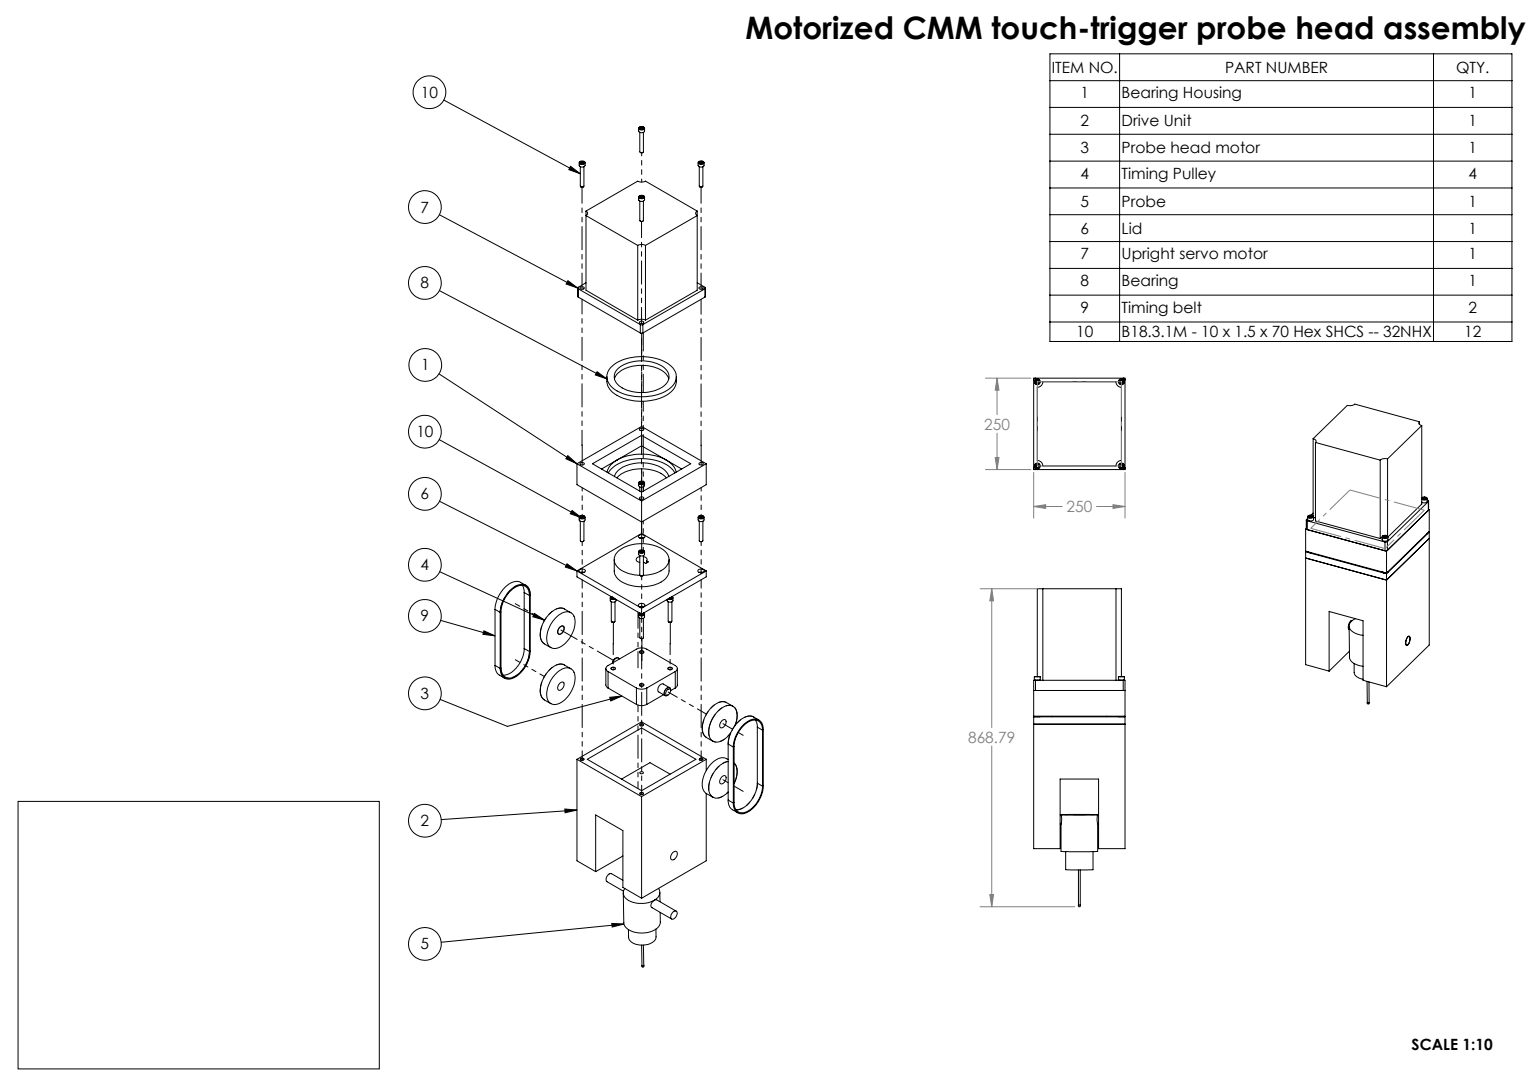
ISO-10303-21;
HEADER;
FILE_DESCRIPTION (('STEP AP214'),
    '1' );
FILE_NAME ('MAT-045',
    '2026-10-28T15:55:38',
    ( '' ),
    ( '' ),
    'SwSTEP 2.0',
    'SolidWorks 2025',
    '' );
FILE_SCHEMA (( 'AUTOMOTIVE_DESIGN' ));
ENDSEC;

DATA;
#1 = CARTESIAN_POINT ( 'NONE',  ( -125.0000000000000000, -125.0000000000000000, 0.000000000000000000 ) ) ;
#2 = ORIENTED_EDGE ( 'NONE', *, *, #4047, .T. ) ;
#3 = CARTESIAN_POINT ( 'NONE',  ( 125.0000000000000000, 52.50000000000000000, 190.0000000000000284 ) ) ;
#4 = LINE ( 'NONE', #7838, #2304 ) ;
#5 = CARTESIAN_POINT ( 'NONE',  ( 0.000000000000000000, 0.000000000000000000, 0.000000000000000000 ) ) ;
#7 = VERTEX_POINT ( 'NONE', #7464 ) ;
#6 = AXIS2_PLACEMENT_3D ( 'NONE', #6964, #1191, #3754 ) ;
#8 = CARTESIAN_POINT ( 'NONE',  ( 120.9999999999999005, 115.0000000000000000, -28.00000000000002487 ) ) ;
#9 = AXIS2_PLACEMENT_3D ( 'NONE', #2697, #3271, #106 ) ;
#10 = DIRECTION ( 'NONE',  ( 0.000000000000000000, -9.256405414277014607E-16, -1.000000000000000000 ) ) ;
#11 = DIRECTION ( 'NONE',  ( 1.000000000000000000, 0.000000000000000000, 0.000000000000000000 ) ) ;
#12 = DIRECTION ( 'NONE',  ( 0.000000000000000000, -0.5000000000000011102, -0.8660254037844379305 ) ) ;
#13 = ORIENTED_EDGE ( 'NONE', *, *, #6011, .T. ) ;
#14 = VERTEX_POINT ( 'NONE', #1674 ) ;
#15 = VERTEX_POINT ( 'NONE', #5559 ) ;
#16 = EDGE_LOOP ( 'NONE', ( #280, #1989 ) ) ;
#17 = CARTESIAN_POINT ( 'NONE',  ( 1.592040838891559490E-15, 125.0000000000000568, 92.99999999999992895 ) ) ;
#18 = ORIENTED_EDGE ( 'NONE', *, *, #6588, .T. ) ;
#19 = ADVANCED_FACE ( 'NONE', ( #8129 ), #7501, .T. ) ;
#20 = DIRECTION ( 'NONE',  ( 0.000000000000000000, 0.000000000000000000, 1.000000000000000000 ) ) ;
#21 = AXIS2_PLACEMENT_3D ( 'NONE', #2988, #8149, #4924 ) ;
#22 = DIRECTION ( 'NONE',  ( -0.000000000000000000, -0.000000000000000000, 1.000000000000000000 ) ) ;
#23 = CARTESIAN_POINT ( 'NONE',  ( 0.000000000000000000, 0.000000000000000000, 20.00000000000000355 ) ) ;
#24 = ITEM_DEFINED_TRANSFORMATION ( 'NONE', 'NONE', #849,  #1299 ) ;
#25 = PLANE ( 'NONE',  #834 ) ;
#26 = AXIS2_PLACEMENT_3D ( 'NONE', #7148, #4607, #975 ) ;
#27 = CARTESIAN_POINT ( 'NONE',  ( -120.0000000000000000, 125.0000000000000000, -28.00000000000002487 ) ) ;
#28 = DIRECTION ( 'NONE',  ( -0.000000000000000000, -1.000000000000000000, 1.586032892321652236E-16 ) ) ;
#29 = ORIENTED_EDGE ( 'NONE', *, *, #180, .F. ) ;
#30 =( REPRESENTATION_RELATIONSHIP ('NONE','NONE', #6882, #239 ) REPRESENTATION_RELATIONSHIP_WITH_TRANSFORMATION ( #3918 )SHAPE_REPRESENTATION_RELATIONSHIP( ) );
#31 = EDGE_CURVE ( 'NONE', #4444, #7082, #3495, .T. ) ;
#32 = CARTESIAN_POINT ( 'NONE',  ( 10.00000000000000000, -3.448762466456902719E-14, 93.74999999999998579 ) ) ;
#33 = ADVANCED_FACE ( 'NONE', ( #7283, #3451 ), #1624, .F. ) ;
#34 = DIRECTION ( 'NONE',  ( -0.8571673007021112234, 1.049727191138617340E-16, 0.5150380749100560429 ) ) ;
#35 = DIRECTION ( 'NONE',  ( 1.000000000000000000, 0.000000000000000000, 0.000000000000000000 ) ) ;
#36 = CYLINDRICAL_SURFACE ( 'NONE', #7648, 95.00000000000001421 ) ;
#37 = DIRECTION ( 'NONE',  ( -0.000000000000000000, -0.000000000000000000, 1.000000000000000000 ) ) ;
#38 = AXIS2_PLACEMENT_3D ( 'NONE', #602, #6938, #1699 ) ;
#39 = CARTESIAN_POINT ( 'NONE',  ( 0.000000000000000000, 7.945337353457666419E-16, -150.0000000000000000 ) ) ;
#40 = ADVANCED_FACE ( 'NONE', ( #3535 ), #4054, .T. ) ;
#41 = DIRECTION ( 'NONE',  ( 1.000000000000000000, 0.000000000000000000, 0.000000000000000000 ) ) ;
#42 = ADVANCED_FACE ( 'NONE', ( #6164, #8163 ), #4942, .F. ) ;
#43 = DIRECTION ( 'NONE',  ( 0.000000000000000000, 0.000000000000000000, 1.000000000000000000 ) ) ;
#44 = ORIENTED_EDGE ( 'NONE', *, *, #3394, .T. ) ;
#45 = CARTESIAN_POINT ( 'NONE',  ( 0.000000000000000000, 0.000000000000000000, 57.99999999999999289 ) ) ;
#46 = APPLICATION_PROTOCOL_DEFINITION ( 'draft international standard', 'automotive_design', 1998, #8017 ) ;
#47 = AXIS2_PLACEMENT_3D ( 'NONE', #5788, #2622, #1664 ) ;
#48 = VERTEX_POINT ( 'NONE', #4805 ) ;
#49 = DIRECTION ( 'NONE',  ( -0.000000000000000000, -0.000000000000000000, 1.000000000000000000 ) ) ;
#50 = VECTOR ( 'NONE', #966, 1000.000000000000000 ) ;
#51 = EDGE_CURVE ( 'NONE', #2241, #1087, #5313, .T. ) ;
#52 = ADVANCED_FACE ( 'NONE', ( #2135 ), #3528, .F. ) ;
#53 = CARTESIAN_POINT ( 'NONE',  ( 54.99999999999999289, -55.00000000000000711, 27.50000000000000000 ) ) ;
#54 = CARTESIAN_POINT ( 'NONE',  ( 115.0000000000000000, 114.9999999999999716, 10.00000000000000000 ) ) ;
#55 = ORIENTED_EDGE ( 'NONE', *, *, #309, .F. ) ;
#56 = LINE ( 'NONE', #2567, #4947 ) ;
#57 = VERTEX_POINT ( 'NONE', #5409 ) ;
#58 = DIRECTION ( 'NONE',  ( 1.000000000000000000, 0.000000000000000000, 0.000000000000000000 ) ) ;
#59 = ORIENTED_EDGE ( 'NONE', *, *, #4247, .T. ) ;
#60 = CARTESIAN_POINT ( 'NONE',  ( -75.00000000000000000, 0.000000000000000000, 0.000000000000000000 ) ) ;
#61 = EDGE_LOOP ( 'NONE', ( #697, #3265, #3475, #7513, #3300, #8064, #2980, #925, #7599, #4514 ) ) ;
#62 = DIRECTION ( 'NONE',  ( -0.000000000000000000, -0.000000000000000000, 1.000000000000000000 ) ) ;
#63 = FACE_OUTER_BOUND ( 'NONE', #5349, .T. ) ;
#64 = CONTEXT_DEPENDENT_SHAPE_REPRESENTATION ( #2778, #4591 ) ;
#65 = CARTESIAN_POINT ( 'NONE',  ( 120.0000000000000000, 125.0000000000000000, -28.00000000000002487 ) ) ;
#66 = VERTEX_POINT ( 'NONE', #5954 ) ;
#67 = VERTEX_POINT ( 'NONE', #6757 ) ;
#68 = PRODUCT_DEFINITION_SHAPE ( 'NONE', 'NONE',  #8365 ) ;
#69 = VECTOR ( 'NONE', #3861, 1000.000000000000000 ) ;
#70 = DIRECTION ( 'NONE',  ( 0.000000000000000000, 0.000000000000000000, -1.000000000000000000 ) ) ;
#71 = ORIENTED_EDGE ( 'NONE', *, *, #7854, .T. ) ;
#72 = ADVANCED_FACE ( 'NONE', ( #4004 ), #7908, .T. ) ;
#73 = DIRECTION ( 'NONE',  ( -1.000000000000000000, -0.000000000000000000, -0.000000000000000000 ) ) ;
#74 = VECTOR ( 'NONE', #8127, 1000.000000000000000 ) ;
#75 = DIRECTION ( 'NONE',  ( -0.000000000000000000, -0.000000000000000000, -1.000000000000000000 ) ) ;
#76 = EDGE_CURVE ( 'NONE', #6243, #2665, #5580, .T. ) ;
#77 = APPLICATION_CONTEXT ( 'automotive_design' ) ;
#78 = LINE ( 'NONE', #2668, #2542 ) ;
#79 = AXIS2_PLACEMENT_3D ( 'NONE', #2314, #7459, #4304 ) ;
#80 = LINE ( 'NONE', #6946, #4020 ) ;
#81 = CARTESIAN_POINT ( 'NONE',  ( 5.000000000000000000, -4.685197434473809430, 7.372574772901430151E-15 ) ) ;
#82 = ORIENTED_EDGE ( 'NONE', *, *, #1098, .T. ) ;
#83 = DIRECTION ( 'NONE',  ( -0.000000000000000000, -1.000000000000000000, 0.000000000000000000 ) ) ;
#84 = CARTESIAN_POINT ( 'NONE',  ( 114.9999999999999716, 114.9999999999999005, 108.4000000000000341 ) ) ;
#85 = ORIENTED_EDGE ( 'NONE', *, *, #3477, .F. ) ;
#86 = CIRCLE ( 'NONE', #779, 5.999999999999984901 ) ;
#87 = ADVANCED_FACE ( 'NONE', ( #1491 ), #7883, .F. ) ;
#88 = AXIS2_PLACEMENT_3D ( 'NONE', #5932, #1987, #3343 ) ;
#89 = ORIENTED_EDGE ( 'NONE', *, *, #6806, .F. ) ;
#90 = CARTESIAN_POINT ( 'NONE',  ( 0.000000000000000000, 4.685197434473814759, -5.637851296924623057E-15 ) ) ;
#91 = DIRECTION ( 'NONE',  ( 1.000000000000000000, 0.000000000000000000, 0.000000000000000000 ) ) ;
#92 = CIRCLE ( 'NONE', #4811, 8.000000000000000000 ) ;
#93 = DIRECTION ( 'NONE',  ( -0.000000000000000000, -1.460819769243626884E-16, -1.000000000000000000 ) ) ;
#94 = SHAPE_REPRESENTATION_RELATIONSHIP ( 'NONE' , 'NONE' ,  #7203, #1812 ) ;
#95 = DIRECTION ( 'NONE',  ( -0.000000000000000000, -0.000000000000000000, 1.000000000000000000 ) ) ;
#96 = ORIENTED_EDGE ( 'NONE', *, *, #4997, .F. ) ;
#97 = ADVANCED_FACE ( 'NONE', ( #330, #202 ), #6713, .F. ) ;
#98 = VECTOR ( 'NONE', #4850, 1000.000000000000000 ) ;
#99 = ORIENTED_EDGE ( 'NONE', *, *, #619, .T. ) ;
#100 = LINE ( 'NONE', #1995, #7998 ) ;
#101 = ORIENTED_EDGE ( 'NONE', *, *, #2517, .F. ) ;
#102 = DIRECTION ( 'NONE',  ( -0.000000000000000000, -0.000000000000000000, 1.000000000000000000 ) ) ;
#103 = FACE_OUTER_BOUND ( 'NONE', #252, .T. ) ;
#104 = VECTOR ( 'NONE', #547, 1000.000000000000000 ) ;
#105 = CIRCLE ( 'NONE', #5900, 5.000000000000004441 ) ;
#106 = DIRECTION ( 'NONE',  ( 1.000000000000000000, 0.000000000000000000, 0.000000000000000000 ) ) ;
#107 = CIRCLE ( 'NONE', #1347, 5.499999999999991118 ) ;
#108 = VECTOR ( 'NONE', #4963, 1000.000000000000000 ) ;
#109 = CARTESIAN_POINT ( 'NONE',  ( -120.0000000000000000, 115.0000000000000000, 340.0000000000000000 ) ) ;
#110 = VERTEX_POINT ( 'NONE', #3400 ) ;
#111 = PRESENTATION_STYLE_ASSIGNMENT (( #1438 ) ) ;
#112 = VECTOR ( 'NONE', #2837, 1000.000000000000000 ) ;
#113 = VECTOR ( 'NONE', #3248, 1000.000000000000000 ) ;
#114 = CARTESIAN_POINT ( 'NONE',  ( -0.8292248493948853882, 50.00000000000000000, -1.010867942207665278E-14 ) ) ;
#115 = FACE_OUTER_BOUND ( 'NONE', #7634, .T. ) ;
#116 = ORIENTED_EDGE ( 'NONE', *, *, #2238, .T. ) ;
#117 = FACE_OUTER_BOUND ( 'NONE', #1113, .T. ) ;
#118 = DIRECTION ( 'NONE',  ( 0.000000000000000000, 0.000000000000000000, -1.000000000000000000 ) ) ;
#119 = AXIS2_PLACEMENT_3D ( 'NONE', #3115, #5695, #7738 ) ;
#120 = CIRCLE ( 'NONE', #6870, 4.999999999999990230 ) ;
#121 = DIRECTION ( 'NONE',  ( -0.000000000000000000, -0.000000000000000000, 1.000000000000000000 ) ) ;
#122 = DIRECTION ( 'NONE',  ( 0.000000000000000000, 0.000000000000000000, -1.000000000000000000 ) ) ;
#123 = FACE_OUTER_BOUND ( 'NONE', #4418, .T. ) ;
#124 = ADVANCED_FACE ( 'NONE', ( #7222 ), #6594, .F. ) ;
#125 = ORIENTED_EDGE ( 'NONE', *, *, #5217, .T. ) ;
#126 = PLANE ( 'NONE',  #6282 ) ;
#127 = DIRECTION ( 'NONE',  ( 0.000000000000000000, 0.000000000000000000, 1.000000000000000000 ) ) ;
#128 = DIRECTION ( 'NONE',  ( 1.000000000000000000, 0.000000000000000000, 0.000000000000000000 ) ) ;
#129 = ORIENTED_EDGE ( 'NONE', *, *, #3717, .T. ) ;
#130 = DIRECTION ( 'NONE',  ( 0.000000000000000000, 0.8660254037844380415, -0.5000000000000011102 ) ) ;
#131 = EDGE_CURVE ( 'NONE', #2948, #8274, #895, .T. ) ;
#132 = SURFACE_SIDE_STYLE ('',( #7319 ) ) ;
#133 = CARTESIAN_POINT ( 'NONE',  ( 14.14213562373095279, -5.000000000000000000, 0.000000000000000000 ) ) ;
#134 = ADVANCED_FACE ( 'NONE', ( #2899 ), #7943, .F. ) ;
#135 = EDGE_CURVE ( 'NONE', #3598, #1656, #3145, .T. ) ;
#136 = CARTESIAN_POINT ( 'NONE',  ( -115.0000000000000142, 115.0000000000000000, 266.9956969048622568 ) ) ;
#137 = ADVANCED_FACE ( 'NONE', ( #4082, #6676, #3444, #6029, #248 ), #2825, .F. ) ;
#138 = EDGE_LOOP ( 'NONE', ( #2116, #5136, #6924, #3116 ) ) ;
#139 = CARTESIAN_POINT ( 'NONE',  ( 9.999999999999998224, 6.613092715395750854E-16, 5.400000000000035882 ) ) ;
#140 = AXIS2_PLACEMENT_3D ( 'NONE', #6010, #7299, #1005 ) ;
#141 = LINE ( 'NONE', #5340, #3208 ) ;
#142 = ORIENTED_EDGE ( 'NONE', *, *, #1025, .T. ) ;
#143 = ORIENTED_EDGE ( 'NONE', *, *, #7822, .F. ) ;
#144 = CARTESIAN_POINT ( 'NONE',  ( -109.5000000000000000, -114.9999999999999858, 20.00000000000000000 ) ) ;
#145 = DIRECTION ( 'NONE',  ( 1.000000000000000000, 0.000000000000000000, 0.000000000000000000 ) ) ;
#146 = DIRECTION ( 'NONE',  ( -1.000000000000000000, -0.000000000000000000, -0.000000000000000000 ) ) ;
#147 = ORIENTED_EDGE ( 'NONE', *, *, #397, .F. ) ;
#148 = AXIS2_PLACEMENT_3D ( 'NONE', #811, #7440, #4371 ) ;
#149 = DIRECTION ( 'NONE',  ( 0.000000000000000000, 0.000000000000000000, 1.000000000000000000 ) ) ;
#150 = ORIENTED_EDGE ( 'NONE', *, *, #4776, .F. ) ;
#151 =( NAMED_UNIT ( * ) PLANE_ANGLE_UNIT ( ) SI_UNIT ( $, .RADIAN. ) );
#152 = EDGE_CURVE ( 'NONE', #6732, #6613, #6071, .T. ) ;
#153 = VERTEX_POINT ( 'NONE', #5449 ) ;
#154 = CARTESIAN_POINT ( 'NONE',  ( -5.558076868459232323, 49.69586384218322905, -1.274058936613796877 ) ) ;
#155 = CIRCLE ( 'NONE', #163, 6.999999999999999112 ) ;
#156 = DIRECTION ( 'NONE',  ( 1.000000000000000000, 0.000000000000000000, 0.000000000000000000 ) ) ;
#157 = ORIENTED_EDGE ( 'NONE', *, *, #4049, .T. ) ;
#158 = PLANE ( 'NONE',  #296 ) ;
#159 = CARTESIAN_POINT ( 'NONE',  ( -114.9999999999999147, 115.0000000000000000, 8.205133554287239938E-16 ) ) ;
#160 = CARTESIAN_POINT ( 'NONE',  ( -125.0000000000000000, -125.0000000000000284, 70.00000000000000000 ) ) ;
#161 = CARTESIAN_POINT ( 'NONE',  ( 5.551115123125782702E-14, 12.49999999999999645, -1.387778780781445676E-14 ) ) ;
#162 = DIRECTION ( 'NONE',  ( 0.000000000000000000, -1.224646799147353207E-16, 1.000000000000000000 ) ) ;
#163 = AXIS2_PLACEMENT_3D ( 'NONE', #406, #5689, #1262 ) ;
#164 = DIRECTION ( 'NONE',  ( 0.000000000000000000, 1.224646799147353207E-16, -1.000000000000000000 ) ) ;
#165 = AXIS2_PLACEMENT_3D ( 'NONE', #5757, #569, #8256 ) ;
#166 = CARTESIAN_POINT ( 'NONE',  ( 124.9999999999997442, -125.0000000000000000, 20.00000000000000000 ) ) ;
#167 = VERTEX_POINT ( 'NONE', #2262 ) ;
#168 = CARTESIAN_POINT ( 'NONE',  ( -120.0000000000000000, 115.0000000000000000, 270.0000000000000000 ) ) ;
#169 = ORIENTED_EDGE ( 'NONE', *, *, #6813, .T. ) ;
#170 = DIRECTION ( 'NONE',  ( 1.000000000000000000, 0.000000000000000000, 0.000000000000000000 ) ) ;
#171 = CARTESIAN_POINT ( 'NONE',  ( 50.00000000000000711, 55.00000000000000000, 220.0000000000000284 ) ) ;
#172 = DIRECTION ( 'NONE',  ( 0.8571673007021112234, 0.000000000000000000, 0.5150380749100560429 ) ) ;
#173 = DIRECTION ( 'NONE',  ( -1.000000000000000000, 0.000000000000000000, 0.000000000000000000 ) ) ;
#174 = CARTESIAN_POINT ( 'NONE',  ( -115.0000000000000000, 115.0000000000000000, 340.0000000000000000 ) ) ;
#175 = AXIS2_PLACEMENT_3D ( 'NONE', #7870, #4041, #5363 ) ;
#176 = LINE ( 'NONE', #2239, #1981 ) ;
#177 = ADVANCED_FACE ( 'NONE', ( #1614 ), #1876, .F. ) ;
#178 = CARTESIAN_POINT ( 'NONE',  ( -10.00000000000000000, 2.291769404546313661E-14, -93.74999999999998579 ) ) ;
#179 = VERTEX_POINT ( 'NONE', #7618 ) ;
#180 = EDGE_CURVE ( 'NONE', #860, #2097, #1404, .T. ) ;
#181 = FACE_OUTER_BOUND ( 'NONE', #3614, .T. ) ;
#182 = ORIENTED_EDGE ( 'NONE', *, *, #917, .F. ) ;
#183 = CARTESIAN_POINT ( 'NONE',  ( -15.00000000000000000, 1.836970198721029589E-15, -120.5000000000000284 ) ) ;
#184 = LINE ( 'NONE', #4786, #3071 ) ;
#185 = VECTOR ( 'NONE', #4186, 1000.000000000000000 ) ;
#186 = CARTESIAN_POINT ( 'NONE',  ( 10.00000000000000000, 54.99999999999989342, 93.75000000000004263 ) ) ;
#187 = DIRECTION ( 'NONE',  ( -0.000000000000000000, -0.000000000000000000, 1.000000000000000000 ) ) ;
#188 = ADVANCED_FACE ( 'NONE', ( #4425 ), #4987, .T. ) ;
#189 = EDGE_CURVE ( 'NONE', #2853, #6262, #8132, .T. ) ;
#190 = EDGE_CURVE ( 'NONE', #8098, #1436, #474, .T. ) ;
#191 = ORIENTED_EDGE ( 'NONE', *, *, #863, .F. ) ;
#192 = DIRECTION ( 'NONE',  ( 1.000000000000000000, 0.000000000000000000, 0.000000000000000000 ) ) ;
#193 = ORIENTED_EDGE ( 'NONE', *, *, #2527, .T. ) ;
#194 = LINE ( 'NONE', #930, #7129 ) ;
#195 = DIRECTION ( 'NONE',  ( 0.8571673007021112234, 0.000000000000000000, 0.5150380749100560429 ) ) ;
#196 = DIRECTION ( 'NONE',  ( -1.000000000000000000, 0.000000000000000000, 0.000000000000000000 ) ) ;
#197 = CARTESIAN_POINT ( 'NONE',  ( 115.0000000000000000, 114.9999999999999716, 10.00000000000000000 ) ) ;
#198 = EDGE_CURVE ( 'NONE', #5389, #4917, #4249, .T. ) ;
#199 = DIRECTION ( 'NONE',  ( -0.000000000000000000, -1.632680918566406547E-16, -1.000000000000000000 ) ) ;
#200 = CARTESIAN_POINT ( 'NONE',  ( 75.00000000000000000, 55.00000000000000711, 27.50000000000000000 ) ) ;
#201 = DIRECTION ( 'NONE',  ( 0.000000000000000000, -0.000000000000000000, 1.000000000000000000 ) ) ;
#202 = FACE_OUTER_BOUND ( 'NONE', #7839, .T. ) ;
#203 = LINE ( 'NONE', #4083, #5436 ) ;
#204 = ADVANCED_FACE ( 'NONE', ( #6375 ), #5709, .F. ) ;
#205 =( GEOMETRIC_REPRESENTATION_CONTEXT ( 3 ) GLOBAL_UNCERTAINTY_ASSIGNED_CONTEXT ( ( #320 ) ) GLOBAL_UNIT_ASSIGNED_CONTEXT ( ( #2718, #3942, #7322 ) ) REPRESENTATION_CONTEXT ( 'NONE', 'WORKASPACE' ) );
#206 = CARTESIAN_POINT ( 'NONE',  ( -31.74999999999995737, 0.000000000000000000, 0.000000000000000000 ) ) ;
#207 = ORIENTED_EDGE ( 'NONE', *, *, #1868, .F. ) ;
#208 = DIRECTION ( 'NONE',  ( -0.000000000000000000, 0.000000000000000000, 1.000000000000000000 ) ) ;
#209 = AXIS2_PLACEMENT_3D ( 'NONE', #1275, #5067, #1401 ) ;
#210 = VERTEX_POINT ( 'NONE', #4338 ) ;
#211 = MECHANICAL_DESIGN_GEOMETRIC_PRESENTATION_REPRESENTATION (  '', ( #3862 ), #2523 ) ;
#212 = CARTESIAN_POINT ( 'NONE',  ( 4.999999999999994671, 0.000000000000000000, 4.057500000000000107 ) ) ;
#213 = CARTESIAN_POINT ( 'NONE',  ( 0.000000000000000000, 2.342598717236902939, -4.057500000000001883 ) ) ;
#214 = DIRECTION ( 'NONE',  ( 1.000000000000000000, 0.000000000000000000, 0.000000000000000000 ) ) ;
#215 = VECTOR ( 'NONE', #34, 1000.000000000000000 ) ;
#216 = DIRECTION ( 'NONE',  ( 0.000000000000000000, 0.000000000000000000, 1.000000000000000000 ) ) ;
#217 = CARTESIAN_POINT ( 'NONE',  ( 17.61817604250836311, 0.000000000000000000, -28.00000000000002487 ) ) ;
#218 = ORIENTED_EDGE ( 'NONE', *, *, #2588, .F. ) ;
#219 = AXIS2_PLACEMENT_3D ( 'NONE', #1415, #5924, #6605 ) ;
#220 = DIRECTION ( 'NONE',  ( 1.000000000000000000, 0.000000000000000000, 0.000000000000000000 ) ) ;
#221 = DIRECTION ( 'NONE',  ( -0.000000000000000000, -0.000000000000000000, 1.000000000000000000 ) ) ;
#222 = AXIS2_PLACEMENT_3D ( 'NONE', #4618, #3222, #5811 ) ;
#223 = ORIENTED_EDGE ( 'NONE', *, *, #4983, .T. ) ;
#224 = CARTESIAN_POINT ( 'NONE',  ( 105.0000000000000000, 8.487013464091010249E-14, 20.00000000000001776 ) ) ;
#225 = CARTESIAN_POINT ( 'NONE',  ( -125.0000000000000000, -125.0000000000000000, 340.0000000000000000 ) ) ;
#226 = EDGE_CURVE ( 'NONE', #3065, #4648, #8287, .T. ) ;
#227 = CONTEXT_DEPENDENT_SHAPE_REPRESENTATION ( #6829, #6951 ) ;
#228 = DIRECTION ( 'NONE',  ( -0.000000000000000000, -0.000000000000000000, 1.000000000000000000 ) ) ;
#229 = VECTOR ( 'NONE', #850, 1000.000000000000000 ) ;
#230 = DIRECTION ( 'NONE',  ( 1.000000000000000000, 0.000000000000000000, 0.000000000000000000 ) ) ;
#231 = CONICAL_SURFACE ( 'NONE', #7932, 4.999999999999990230, 1.029744258676656754 ) ;
#232 = ORIENTED_EDGE ( 'NONE', *, *, #4651, .F. ) ;
#233 = PRODUCT_DEFINITION_CONTEXT ( 'detailed design', #2370, 'design' ) ;
#234 = EDGE_LOOP ( 'NONE', ( #3769, #1956 ) ) ;
#235 = DIRECTION ( 'NONE',  ( 1.000000000000000000, 0.000000000000000000, 0.000000000000000000 ) ) ;
#236 = CIRCLE ( 'NONE', #5782, 12.50000000000000000 ) ;
#237 = ORIENTED_EDGE ( 'NONE', *, *, #6341, .T. ) ;
#238 = CARTESIAN_POINT ( 'NONE',  ( 4.999999999999994671, 0.000000000000000000, 0.000000000000000000 ) ) ;
#239 = SHAPE_REPRESENTATION ( 'socket head cap screw_am_B18.3.1M - 10 x 1.5 x 70 Hex SHCS -- 32NHX', ( #1299 ), #3819 ) ;
#240 = EDGE_CURVE ( 'NONE', #3849, #6134, #2101, .T. ) ;
#241 = EDGE_CURVE ( 'NONE', #7110, #7555, #6784, .T. ) ;
#242 = CARTESIAN_POINT ( 'NONE',  ( 8.253058034503027329, 49.31520865873546455, -3.102932425833026642 ) ) ;
#243 = CIRCLE ( 'NONE', #6316, 15.00000000000001421 ) ;
#244 = CIRCLE ( 'NONE', #3336, 5.999999999999991118 ) ;
#245 = LINE ( 'NONE', #5564, #6769 ) ;
#246 = FACE_OUTER_BOUND ( 'NONE', #495, .T. ) ;
#247 = CARTESIAN_POINT ( 'NONE',  ( 55.00000000000000000, 55.00000000000000000, 240.0000000000000284 ) ) ;
#248 = FACE_OUTER_BOUND ( 'NONE', #5521, .T. ) ;
#249 = LINE ( 'NONE', #7309, #1348 ) ;
#250 = CONICAL_SURFACE ( 'NONE', #6332, 6.999999999999999112, 0.7853981633974482790 ) ;
#251 = DIRECTION ( 'NONE',  ( 1.000000000000000000, 0.000000000000000000, 0.000000000000000000 ) ) ;
#252 = EDGE_LOOP ( 'NONE', ( #5794, #5594, #8327, #2636 ) ) ;
#253 = VECTOR ( 'NONE', #4816, 1000.000000000000000 ) ;
#254 = ORIENTED_EDGE ( 'NONE', *, *, #2828, .T. ) ;
#255 = CIRCLE ( 'NONE', #5116, 12.99999999999999822 ) ;
#256 = DIRECTION ( 'NONE',  ( -1.000000000000000000, -1.321694076934710155E-16, 0.000000000000000000 ) ) ;
#257 = LINE ( 'NONE', #1580, #7553 ) ;
#258 = ADVANCED_FACE ( 'NONE', ( #117 ), #4551, .F. ) ;
#259 = DIRECTION ( 'NONE',  ( 9.992007221626408864E-16, 1.000000000000000000, 0.000000000000000000 ) ) ;
#260 = VECTOR ( 'NONE', #1303, 1000.000000000000000 ) ;
#261 = DIRECTION ( 'NONE',  ( -0.000000000000000000, -0.000000000000000000, -1.000000000000000000 ) ) ;
#262 = DIRECTION ( 'NONE',  ( -0.000000000000000000, -0.000000000000000000, 1.000000000000000000 ) ) ;
#263 = DIRECTION ( 'NONE',  ( -0.000000000000000000, -7.945337353457666666E-18, -1.000000000000000000 ) ) ;
#264 = EDGE_LOOP ( 'NONE', ( #6496, #2959, #7689, #1000 ) ) ;
#265 = DIRECTION ( 'NONE',  ( 0.000000000000000000, 0.000000000000000000, -1.000000000000000000 ) ) ;
#266 = LINE ( 'NONE', #3462, #5375 ) ;
#267 = ORIENTED_EDGE ( 'NONE', *, *, #1486, .F. ) ;
#268 = VERTEX_POINT ( 'NONE', #3361 ) ;
#269 = CARTESIAN_POINT ( 'NONE',  ( 121.0000000000000284, -115.0000000000000000, 20.00000000000000355 ) ) ;
#270 = FACE_OUTER_BOUND ( 'NONE', #1601, .T. ) ;
#271 = CARTESIAN_POINT ( 'NONE',  ( 0.000000000000000000, -4.500000000000000000, -118.0000000000000284 ) ) ;
#272 = DIRECTION ( 'NONE',  ( 1.000000000000000000, 0.000000000000000000, 0.000000000000000000 ) ) ;
#273 = ORIENTED_EDGE ( 'NONE', *, *, #5206, .F. ) ;
#274 = DIRECTION ( 'NONE',  ( 0.000000000000000000, -0.000000000000000000, -1.000000000000000000 ) ) ;
#275 = ORIENTED_EDGE ( 'NONE', *, *, #5871, .F. ) ;
#276 = CARTESIAN_POINT ( 'NONE',  ( -104.9999999999999432, -105.0000000000000853, 240.0000000000000284 ) ) ;
#277 = AXIS2_PLACEMENT_3D ( 'NONE', #5185, #677, #1430 ) ;
#278 = CARTESIAN_POINT ( 'NONE',  ( 115.0000000000000426, -115.0000000000002558, -1.599999999999995426 ) ) ;
#279 = CARTESIAN_POINT ( 'NONE',  ( 0.000000000000000000, 72.49999999999995737, 66.99999999999994316 ) ) ;
#280 = ORIENTED_EDGE ( 'NONE', *, *, #241, .T. ) ;
#281 = CARTESIAN_POINT ( 'NONE',  ( 0.000000000000000000, 50.00000000000000000, 0.000000000000000000 ) ) ;
#282 = DIRECTION ( 'NONE',  ( -0.000000000000000000, 1.000000000000000000, 2.960594732333750610E-16 ) ) ;
#283 = ADVANCED_FACE ( 'NONE', ( #3284, #3966, #689, #5244, #1367, #6459 ), #5952, .F. ) ;
#284 = EDGE_CURVE ( 'NONE', #5879, #3698, #7868, .T. ) ;
#285 = CARTESIAN_POINT ( 'NONE',  ( 10.00000000000000000, -3.448762466456902719E-14, 93.74999999999998579 ) ) ;
#286 = EDGE_CURVE ( 'NONE', #441, #1522, #6503, .T. ) ;
#287 = CARTESIAN_POINT ( 'NONE',  ( 110.0000000000000142, -115.0000000000000000, 270.0000000000000000 ) ) ;
#288 = DIRECTION ( 'NONE',  ( 0.000000000000000000, 0.000000000000000000, 1.000000000000000000 ) ) ;
#289 = CIRCLE ( 'NONE', #5015, 12.99999999999999822 ) ;
#290 = ORIENTED_EDGE ( 'NONE', *, *, #7886, .F. ) ;
#291 = FILL_AREA_STYLE ('',( #6798 ) ) ;
#292 = ORIENTED_EDGE ( 'NONE', *, *, #3848, .F. ) ;
#293 = VERTEX_POINT ( 'NONE', #814 ) ;
#294 = ORIENTED_EDGE ( 'NONE', *, *, #3089, .F. ) ;
#295 = EDGE_CURVE ( 'NONE', #2535, #179, #3684, .T. ) ;
#296 = AXIS2_PLACEMENT_3D ( 'NONE', #5951, #1969, #3246 ) ;
#297 = PLANE ( 'NONE',  #642 ) ;
#298 = AXIS2_PLACEMENT_3D ( 'NONE', #2191, #4194, #6554 ) ;
#299 = APPLICATION_CONTEXT ( 'automotive_design' ) ;
#300 = CARTESIAN_POINT ( 'NONE',  ( -114.9999999999999147, 115.0000000000000000, 0.000000000000000000 ) ) ;
#301 = ORIENTED_EDGE ( 'NONE', *, *, #715, .F. ) ;
#302 =( NAMED_UNIT ( * ) SI_UNIT ( $, .STERADIAN. ) SOLID_ANGLE_UNIT ( ) );
#303 = CARTESIAN_POINT ( 'NONE',  ( 0.000000000000000000, 125.0000000000000568, 79.99999999999992895 ) ) ;
#304 = DIRECTION ( 'NONE',  ( -0.000000000000000000, -0.000000000000000000, 1.000000000000000000 ) ) ;
#305 = CARTESIAN_POINT ( 'NONE',  ( 10.00000000000000000, -57.99999999999995737, -93.75000000000001421 ) ) ;
#306 = VERTEX_POINT ( 'NONE', #4470 ) ;
#307 = PLANE ( 'NONE',  #7987 ) ;
#308 = EDGE_CURVE ( 'NONE', #902, #5541, #1677, .T. ) ;
#309 = EDGE_CURVE ( 'NONE', #7487, #6953, #643, .T. ) ;
#310 = CLOSED_SHELL ( 'NONE', ( #3649, #1499, #7471, #6289, #6383, #2621, #654, #8259, #5840, #40, #7066, #4000, #7991, #7178, #2940, #72, #5941, #5722, #5455, #6114, #6194, #3420, #920, #177, #2590, #2030, #4073, #5503, #4001, #3296, #1919, #610, #4469, #5040, #3468, #42, #666, #5099, #4929, #6667, #3666 ) ) ;
#311 = PLANE ( 'NONE',  #4412 ) ;
#312 = EDGE_LOOP ( 'NONE', ( #3163, #5141 ) ) ;
#313 = DIRECTION ( 'NONE',  ( -0.000000000000000000, -0.000000000000000000, 1.000000000000000000 ) ) ;
#314 = VERTEX_POINT ( 'NONE', #6672 ) ;
#315 = CARTESIAN_POINT ( 'NONE',  ( 0.000000000000000000, 0.000000000000000000, -128.0000000000000284 ) ) ;
#316 = CARTESIAN_POINT ( 'NONE',  ( 54.99999999999999289, 55.00000000000000711, 27.50000000000000000 ) ) ;
#317 = CARTESIAN_POINT ( 'NONE',  ( 125.0000000000000000, 125.0000000000000000, 0.000000000000000000 ) ) ;
#318 = CARTESIAN_POINT ( 'NONE',  ( 115.0000000000000284, -115.0000000000000000, 20.00000000000000355 ) ) ;
#319 = CIRCLE ( 'NONE', #6386, 95.00000000000001421 ) ;
#320 = UNCERTAINTY_MEASURE_WITH_UNIT (LENGTH_MEASURE( 1.000000000000000082E-05 ), #2718, 'distance_accuracy_value', 'NONE');
#321 = VERTEX_POINT ( 'NONE', #4199 ) ;
#322 = DIRECTION ( 'NONE',  ( -0.000000000000000000, -0.000000000000000000, -1.000000000000000000 ) ) ;
#323 = VERTEX_POINT ( 'NONE', #4680 ) ;
#324 = CYLINDRICAL_SURFACE ( 'NONE', #1742, 5.999999999999991118 ) ;
#325 = DIRECTION ( 'NONE',  ( 1.000000000000000000, 0.000000000000000000, 0.000000000000000000 ) ) ;
#326 = VERTEX_POINT ( 'NONE', #1488 ) ;
#327 = CARTESIAN_POINT ( 'NONE',  ( 11.38744771879169093, 48.68625849413228934, -7.328777110660809946 ) ) ;
#328 = DIRECTION ( 'NONE',  ( 0.000000000000000000, 0.000000000000000000, -1.000000000000000000 ) ) ;
#329 = CARTESIAN_POINT ( 'NONE',  ( 120.0000000000000000, -115.0000000000000000, 270.0000000000000000 ) ) ;
#330 = FACE_BOUND ( 'NONE', #1932, .T. ) ;
#331 = LINE ( 'NONE', #1063, #1617 ) ;
#332 = ORIENTED_EDGE ( 'NONE', *, *, #3253, .T. ) ;
#333 = CARTESIAN_POINT ( 'NONE',  ( 125.0000000000000000, 52.50000000000000000, 190.0000000000000284 ) ) ;
#334 = VERTEX_POINT ( 'NONE', #4039 ) ;
#335 = EDGE_CURVE ( 'NONE', #1946, #314, #6628, .T. ) ;
#336 = ORIENTED_EDGE ( 'NONE', *, *, #3022, .F. ) ;
#337 = CARTESIAN_POINT ( 'NONE',  ( 10.00000000000000000, -57.99999999999995737, -93.75000000000001421 ) ) ;
#338 = AXIS2_PLACEMENT_3D ( 'NONE', #4056, #6518, #5262 ) ;
#339 = CARTESIAN_POINT ( 'NONE',  ( -75.00000000000000000, -75.00000000000000000, -27.50000000000000000 ) ) ;
#340 = ORIENTED_EDGE ( 'NONE', *, *, #1134, .T. ) ;
#341 = CARTESIAN_POINT ( 'NONE',  ( -8.253058034503022000, -49.31520865873545034, -3.102932425833025309 ) ) ;
#342 =( NAMED_UNIT ( * ) SI_UNIT ( $, .STERADIAN. ) SOLID_ANGLE_UNIT ( ) );
#343 = ADVANCED_FACE ( 'NONE', ( #2220 ), #2779, .T. ) ;
#344 = CARTESIAN_POINT ( 'NONE',  ( 115.0000000000000000, 115.0000000000000000, 270.0000000000000000 ) ) ;
#345 = DIRECTION ( 'NONE',  ( -0.000000000000000000, 1.000000000000000000, 1.224646799147353207E-16 ) ) ;
#346 = EDGE_LOOP ( 'NONE', ( #3800, #3054, #6759, #1115 ) ) ;
#347 = DIRECTION ( 'NONE',  ( -1.000000000000000000, 0.000000000000000000, -0.000000000000000000 ) ) ;
#348 = CARTESIAN_POINT ( 'NONE',  ( -115.0000000000000000, 115.0000000000000000, 340.0000000000000000 ) ) ;
#349 = ORIENTED_EDGE ( 'NONE', *, *, #2079, .F. ) ;
#350 = AXIS2_PLACEMENT_3D ( 'NONE', #7544, #3683, #6944 ) ;
#351 = VERTEX_POINT ( 'NONE', #1784 ) ;
#352 = DIRECTION ( 'NONE',  ( 1.000000000000000000, 0.000000000000000000, 0.000000000000000000 ) ) ;
#353 = DIRECTION ( 'NONE',  ( 1.000000000000000000, 0.000000000000000000, 0.000000000000000000 ) ) ;
#354 = VERTEX_POINT ( 'NONE', #1827 ) ;
#355 = CARTESIAN_POINT ( 'NONE',  ( -110.0000000000000142, -115.0000000000000000, 270.0000000000000000 ) ) ;
#356 = AXIS2_PLACEMENT_3D ( 'NONE', #3494, #2749, #5417 ) ;
#357 = ORIENTED_EDGE ( 'NONE', *, *, #7077, .F. ) ;
#358 = ORIENTED_EDGE ( 'NONE', *, *, #5305, .F. ) ;
#359 = LINE ( 'NONE', #1094, #4691 ) ;
#360 = ORIENTED_EDGE ( 'NONE', *, *, #2100, .T. ) ;
#361 = DIRECTION ( 'NONE',  ( 1.000000000000000000, 0.000000000000000000, 0.000000000000000000 ) ) ;
#362 = ORIENTED_EDGE ( 'NONE', *, *, #3599, .T. ) ;
#363 = CARTESIAN_POINT ( 'NONE',  ( 115.0000000000000000, 115.0000000000000000, 70.00000000000000000 ) ) ;
#364 = AXIS2_PLACEMENT_3D ( 'NONE', #8155, #2383, #3917 ) ;
#365 = ORIENTED_EDGE ( 'NONE', *, *, #7229, .F. ) ;
#366 = DIRECTION ( 'NONE',  ( -0.000000000000000000, 1.000000000000000000, -0.000000000000000000 ) ) ;
#367 = VECTOR ( 'NONE', #3652, 1000.000000000000000 ) ;
#368 = ORIENTED_EDGE ( 'NONE', *, *, #2100, .F. ) ;
#369 = CARTESIAN_POINT ( 'NONE',  ( 20.76917701662883076, -5.000000000000000000, 0.000000000000000000 ) ) ;
#370 = CARTESIAN_POINT ( 'NONE',  ( 0.000000000000000000, 0.000000000000000000, -120.5000000000000284 ) ) ;
#371 = AXIS2_PLACEMENT_3D ( 'NONE', #2070, #6035, #7190 ) ;
#372 = VERTEX_POINT ( 'NONE', #4240 ) ;
#373 = CARTESIAN_POINT ( 'NONE',  ( 1.592040838891560279E-15, -125.0000000000000568, 92.99999999999997158 ) ) ;
#374 = EDGE_LOOP ( 'NONE', ( #2417, #694, #4640, #1560, #2095 ) ) ;
#375 = ORIENTED_EDGE ( 'NONE', *, *, #4047, .F. ) ;
#376 = VECTOR ( 'NONE', #1952, 1000.000000000000000 ) ;
#377 = AXIS2_PLACEMENT_3D ( 'NONE', #5650, #8275, #3063 ) ;
#378 = VERTEX_POINT ( 'NONE', #1356 ) ;
#379 = ORIENTED_EDGE ( 'NONE', *, *, #688, .F. ) ;
#380 = DIRECTION ( 'NONE',  ( -1.000000000000000000, 0.000000000000000000, 0.000000000000000000 ) ) ;
#381 = VERTEX_POINT ( 'NONE', #27 ) ;
#382 = CARTESIAN_POINT ( 'NONE',  ( -54.99999999999999289, 55.00000000000000711, 27.50000000000000000 ) ) ;
#383 = AXIS2_PLACEMENT_3D ( 'NONE', #486, #7032, #3735 ) ;
#384 = CIRCLE ( 'NONE', #1751, 5.999999999999984901 ) ;
#385 = EDGE_CURVE ( 'NONE', #378, #1211, #7861, .T. ) ;
#386 = CARTESIAN_POINT ( 'NONE',  ( 105.0000000000000000, -105.0000000000000568, 240.0000000000000284 ) ) ;
#387 = VECTOR ( 'NONE', #1755, 1000.000000000000000 ) ;
#388 = ORIENTED_EDGE ( 'NONE', *, *, #3277, .T. ) ;
#389 = DIRECTION ( 'NONE',  ( -0.000000000000000000, -0.000000000000000000, 1.000000000000000000 ) ) ;
#390 = AXIS2_PLACEMENT_3D ( 'NONE', #5966, #1418, #2752 ) ;
#391 = VECTOR ( 'NONE', #4376, 1000.000000000000000 ) ;
#392 = ORIENTED_EDGE ( 'NONE', *, *, #1590, .F. ) ;
#393 = ADVANCED_FACE ( 'NONE', ( #3838 ), #3197, .T. ) ;
#394 = DIRECTION ( 'NONE',  ( 0.000000000000000000, 0.000000000000000000, 1.000000000000000000 ) ) ;
#395 = DIRECTION ( 'NONE',  ( -0.000000000000000000, -0.000000000000000000, 1.000000000000000000 ) ) ;
#396 = EDGE_CURVE ( 'NONE', #4375, #2961, #3878, .T. ) ;
#397 = EDGE_CURVE ( 'NONE', #2572, #1918, #4635, .T. ) ;
#398 = DIRECTION ( 'NONE',  ( 0.000000000000000000, 0.000000000000000000, 1.000000000000000000 ) ) ;
#399 = ORIENTED_EDGE ( 'NONE', *, *, #419, .F. ) ;
#400 = LINE ( 'NONE', #8042, #670 ) ;
#401 = CARTESIAN_POINT ( 'NONE',  ( 1.632468168883557169, -49.97996006834705440, -24.92059050027006606 ) ) ;
#402 = VERTEX_POINT ( 'NONE', #4592 ) ;
#403 = PRESENTATION_STYLE_ASSIGNMENT (( #6315 ) ) ;
#404 = CYLINDRICAL_SURFACE ( 'NONE', #1048, 54.99999999999995026 ) ;
#405 = ORIENTED_EDGE ( 'NONE', *, *, #8301, .F. ) ;
#406 = CARTESIAN_POINT ( 'NONE',  ( 0.000000000000000000, 0.000000000000000000, 0.000000000000000000 ) ) ;
#407 = ORIENTED_EDGE ( 'NONE', *, *, #3693, .F. ) ;
#408 = DIRECTION ( 'NONE',  ( 0.000000000000000000, -1.000000000000000000, 0.000000000000000000 ) ) ;
#409 = ORIENTED_EDGE ( 'NONE', *, *, #5829, .F. ) ;
#410 = FACE_OUTER_BOUND ( 'NONE', #2022, .T. ) ;
#411 = LINE ( 'NONE', #3703, #3911 ) ;
#412 = APPLICATION_PROTOCOL_DEFINITION ( 'draft international standard', 'automotive_design', 1998, #7867 ) ;
#413 = CIRCLE ( 'NONE', #1506, 4.057500000000000107 ) ;
#414 = ORIENTED_EDGE ( 'NONE', *, *, #7854, .F. ) ;
#415 = FACE_OUTER_BOUND ( 'NONE', #707, .T. ) ;
#416 = VERTEX_POINT ( 'NONE', #5187 ) ;
#417 = PLANE ( 'NONE',  #21 ) ;
#418 = ORIENTED_EDGE ( 'NONE', *, *, #1413, .T. ) ;
#419 = EDGE_CURVE ( 'NONE', #3125, #7541, #3274, .T. ) ;
#420 = CARTESIAN_POINT ( 'NONE',  ( -102.5000000000000000, 0.000000000000000000, -9.500000000000008882 ) ) ;
#421 = VECTOR ( 'NONE', #7428, 1000.000000000000000 ) ;
#422 = DIRECTION ( 'NONE',  ( -0.000000000000000000, -1.000000000000000000, -1.224646799147353207E-16 ) ) ;
#423 = CARTESIAN_POINT ( 'NONE',  ( 0.000000000000000000, 1.191800603018649864E-15, -100.0000000000000000 ) ) ;
#424 = ORIENTED_EDGE ( 'NONE', *, *, #8219, .F. ) ;
#425 =( LENGTH_UNIT ( ) NAMED_UNIT ( * ) SI_UNIT ( .MILLI., .METRE. ) );
#426 = VERTEX_POINT ( 'NONE', #6449 ) ;
#427 = ORIENTED_EDGE ( 'NONE', *, *, #5038, .F. ) ;
#428 = LINE ( 'NONE', #8161, #3975 ) ;
#429 = PLANE ( 'NONE',  #5764 ) ;
#430 = CARTESIAN_POINT ( 'NONE',  ( 114.9999999999999147, 115.0000000000000000, 0.000000000000000000 ) ) ;
#431 = VERTEX_POINT ( 'NONE', #681 ) ;
#432 = CARTESIAN_POINT ( 'NONE',  ( 124.0000000000000000, 114.9999999999999716, 10.00000000000000000 ) ) ;
#433 = EDGE_LOOP ( 'NONE', ( #2336, #6110, #4542, #3751 ) ) ;
#434 = CIRCLE ( 'NONE', #1525, 0.4000000000000001887 ) ;
#435 = EDGE_LOOP ( 'NONE', ( #3516, #6927 ) ) ;
#436 = DIRECTION ( 'NONE',  ( -1.000000000000000000, -0.000000000000000000, -0.000000000000000000 ) ) ;
#437 = DIRECTION ( 'NONE',  ( 0.000000000000000000, 0.000000000000000000, -1.000000000000000000 ) ) ;
#438 = ORIENTED_EDGE ( 'NONE', *, *, #5217, .F. ) ;
#439 = DIRECTION ( 'NONE',  ( -0.000000000000000000, -0.000000000000000000, 1.000000000000000000 ) ) ;
#440 = CARTESIAN_POINT ( 'NONE',  ( 1.592040838891560279E-15, -52.49999999999996447, 92.99999999999995737 ) ) ;
#441 = VERTEX_POINT ( 'NONE', #3239 ) ;
#442 = LINE ( 'NONE', #6912, #6022 ) ;
#443 = EDGE_CURVE ( 'NONE', #5909, #448, #7758, .T. ) ;
#444 = EDGE_CURVE ( 'NONE', #3837, #3210, #4518, .T. ) ;
#445 = DIRECTION ( 'NONE',  ( 0.000000000000000000, 0.000000000000000000, 1.000000000000000000 ) ) ;
#446 = ORIENTED_EDGE ( 'NONE', *, *, #1545, .T. ) ;
#447 = AXIS2_PLACEMENT_3D ( 'NONE', #5326, #6108, #2222 ) ;
#448 = VERTEX_POINT ( 'NONE', #171 ) ;
#449 = DIRECTION ( 'NONE',  ( -1.000000000000000000, 0.000000000000000000, -0.000000000000000000 ) ) ;
#450 = DIRECTION ( 'NONE',  ( -1.000000000000000000, 0.000000000000000000, 0.000000000000000000 ) ) ;
#451 = DIRECTION ( 'NONE',  ( -1.000000000000000000, 0.000000000000000000, -0.000000000000000000 ) ) ;
#452 = ORIENTED_EDGE ( 'NONE', *, *, #385, .T. ) ;
#453 = CARTESIAN_POINT ( 'NONE',  ( -75.00000000000000000, 55.00000000000000711, 27.50000000000000000 ) ) ;
#454 = ADVANCED_FACE ( 'NONE', ( #1334 ), #2234, .F. ) ;
#455 = PLANE ( 'NONE',  #2955 ) ;
#456 = ORIENTED_EDGE ( 'NONE', *, *, #6488, .T. ) ;
#457 = AXIS2_PLACEMENT_3D ( 'NONE', #8109, #6795, #201 ) ;
#458 = APPLICATION_PROTOCOL_DEFINITION ( 'draft international standard', 'automotive_design', 1998, #3360 ) ;
#459 = DIRECTION ( 'NONE',  ( 1.000000000000000000, 0.000000000000000000, 0.000000000000000000 ) ) ;
#460 = EDGE_CURVE ( 'NONE', #4967, #5007, #866, .T. ) ;
#461 = EDGE_CURVE ( 'NONE', #1211, #7416, #1823, .T. ) ;
#462 = EDGE_CURVE ( 'NONE', #1143, #501, #4654, .T. ) ;
#463 = ORIENTED_EDGE ( 'NONE', *, *, #6488, .F. ) ;
#464 =( GEOMETRIC_REPRESENTATION_CONTEXT ( 3 ) GLOBAL_UNCERTAINTY_ASSIGNED_CONTEXT ( ( #4359 ) ) GLOBAL_UNIT_ASSIGNED_CONTEXT ( ( #3691, #7766, #3944 ) ) REPRESENTATION_CONTEXT ( 'NONE', 'WORKASPACE' ) );
#465 = CARTESIAN_POINT ( 'NONE',  ( -120.0000000000000000, -125.0000000000000000, 0.000000000000000000 ) ) ;
#466 = EDGE_LOOP ( 'NONE', ( #8090, #6345 ) ) ;
#467 = CARTESIAN_POINT ( 'NONE',  ( 0.000000000000000000, 72.49999999999995737, 79.99999999999994316 ) ) ;
#468 = CYLINDRICAL_SURFACE ( 'NONE', #7813, 12.99999999999999822 ) ;
#469 = VERTEX_POINT ( 'NONE', #7667 ) ;
#470 = EDGE_CURVE ( 'NONE', #8314, #877, #319, .T. ) ;
#471 = VERTEX_POINT ( 'NONE', #3527 ) ;
#472 =( REPRESENTATION_RELATIONSHIP ('NONE','NONE', #6882, #3965 ) REPRESENTATION_RELATIONSHIP_WITH_TRANSFORMATION ( #8321 )SHAPE_REPRESENTATION_RELATIONSHIP( ) );
#473 = EDGE_LOOP ( 'NONE', ( #7850, #7709, #1051, #6786 ) ) ;
#474 = LINE ( 'NONE', #5587, #3002 ) ;
#475 = FACE_OUTER_BOUND ( 'NONE', #6736, .T. ) ;
#476 = PRODUCT_DEFINITION_SHAPE ( 'NONE', 'NONE',  #8369 ) ;
#477 = FACE_OUTER_BOUND ( 'NONE', #2938, .T. ) ;
#478 = EDGE_LOOP ( 'NONE', ( #2078, #3169, #678, #44 ) ) ;
#479 = CARTESIAN_POINT ( 'NONE',  ( -11.83759003446072811, -48.57866412327431505, -8.463974912767858072 ) ) ;
#480 = EDGE_LOOP ( 'NONE', ( #1640, #5852, #3435, #5019 ) ) ;
#481 = ORIENTED_EDGE ( 'NONE', *, *, #4733, .F. ) ;
#482 = CIRCLE ( 'NONE', #7640, 8.999999999999994671 ) ;
#483 = CARTESIAN_POINT ( 'NONE',  ( -10.00000000000000000, 2.291769404546313661E-14, -93.74999999999998579 ) ) ;
#484 = CARTESIAN_POINT ( 'NONE',  ( 0.000000000000000000, 37.49999999999999289, -150.0000000000000000 ) ) ;
#485 = EDGE_LOOP ( 'NONE', ( #1792, #6365 ) ) ;
#486 = CARTESIAN_POINT ( 'NONE',  ( -114.9999999999999147, -115.0000000000000000, 250.0000000000000000 ) ) ;
#487 = DIRECTION ( 'NONE',  ( 1.000000000000000000, 0.000000000000000000, 0.000000000000000000 ) ) ;
#488 =( GEOMETRIC_REPRESENTATION_CONTEXT ( 3 ) GLOBAL_UNCERTAINTY_ASSIGNED_CONTEXT ( ( #3697 ) ) GLOBAL_UNIT_ASSIGNED_CONTEXT ( ( #6897, #8033, #302 ) ) REPRESENTATION_CONTEXT ( 'NONE', 'WORKASPACE' ) );
#489 = FACE_BOUND ( 'NONE', #5526, .T. ) ;
#490 = LINE ( 'NONE', #5647, #5836 ) ;
#491 = UNCERTAINTY_MEASURE_WITH_UNIT (LENGTH_MEASURE( 1.000000000000000082E-05 ), #6982, 'distance_accuracy_value', 'NONE');
#492 = ORIENTED_EDGE ( 'NONE', *, *, #5575, .T. ) ;
#493 = DIRECTION ( 'NONE',  ( -0.000000000000000000, -0.000000000000000000, 1.000000000000000000 ) ) ;
#494 = CARTESIAN_POINT ( 'NONE',  ( -75.00000000000000000, 1.530808498934191521E-15, -12.50000000000000000 ) ) ;
#495 = EDGE_LOOP ( 'NONE', ( #2773, #191, #1926, #6706 ) ) ;
#496 = ADVANCED_FACE ( 'NONE', ( #6675 ), #5448, .T. ) ;
#497 = CARTESIAN_POINT ( 'NONE',  ( 10.00000000000000000, -3.448762466456902719E-14, 148.7499999999999432 ) ) ;
#498 = DIRECTION ( 'NONE',  ( -1.000000000000000000, -0.000000000000000000, -0.000000000000000000 ) ) ;
#499 = ORIENTED_EDGE ( 'NONE', *, *, #1382, .F. ) ;
#500 = APPLICATION_PROTOCOL_DEFINITION ( 'draft international standard', 'automotive_design', 1998, #7435 ) ;
#501 = VERTEX_POINT ( 'NONE', #1652 ) ;
#502 = DIRECTION ( 'NONE',  ( 0.000000000000000000, 0.000000000000000000, 1.000000000000000000 ) ) ;
#503 = DIRECTION ( 'NONE',  ( 1.000000000000000000, 1.321694076934710648E-16, 0.000000000000000000 ) ) ;
#504 = AXIS2_PLACEMENT_3D ( 'NONE', #7381, #3470, #967 ) ;
#505 = EDGE_CURVE ( 'NONE', #48, #4486, #8022, .T. ) ;
#506 = CARTESIAN_POINT ( 'NONE',  ( 17.61817604250836311, 0.000000000000000000, -128.0000120000000265 ) ) ;
#507 = AXIS2_PLACEMENT_3D ( 'NONE', #6558, #3976, #170 ) ;
#508 = ORIENTED_EDGE ( 'NONE', *, *, #4848, .F. ) ;
#509 = VERTEX_POINT ( 'NONE', #329 ) ;
#510 = EDGE_CURVE ( 'NONE', #4072, #3309, #2872, .T. ) ;
#511 = DIRECTION ( 'NONE',  ( 0.000000000000000000, 0.5000000000000011102, 0.8660254037844380415 ) ) ;
#512 = EDGE_CURVE ( 'NONE', #554, #2252, #3311, .T. ) ;
#513 = DIRECTION ( 'NONE',  ( -0.000000000000000000, -0.000000000000000000, 1.000000000000000000 ) ) ;
#514 = ORIENTED_EDGE ( 'NONE', *, *, #1744, .T. ) ;
#515 = ORIENTED_EDGE ( 'NONE', *, *, #1831, .T. ) ;
#516 = AXIS2_PLACEMENT_3D ( 'NONE', #7483, #1692, #2897 ) ;
#517 = ORIENTED_EDGE ( 'NONE', *, *, #3189, .F. ) ;
#518 = FACE_OUTER_BOUND ( 'NONE', #6089, .T. ) ;
#519 = CONICAL_SURFACE ( 'NONE', #3466, 5.999999999999991118, 1.029744258676652313 ) ;
#520 = LINE ( 'NONE', #6379, #1616 ) ;
#521 = ORIENTED_EDGE ( 'NONE', *, *, #5929, .F. ) ;
#522 = CARTESIAN_POINT ( 'NONE',  ( -3.257728639534228865, -49.90026920665918198, -24.59591892738197672 ) ) ;
#523 = APPLICATION_CONTEXT ( 'automotive_design' ) ;
#524 = ORIENTED_EDGE ( 'NONE', *, *, #1693, .T. ) ;
#525 = CIRCLE ( 'NONE', #6324, 4.999999999999990230 ) ;
#526 = CARTESIAN_POINT ( 'NONE',  ( 0.000000000000000000, 7.945337353457666419E-16, -150.0000000000000000 ) ) ;
#527 = CARTESIAN_POINT ( 'NONE',  ( 54.99999999999999289, -55.00000000000000711, -27.50000000000000000 ) ) ;
#528 = CARTESIAN_POINT ( 'NONE',  ( -55.00000000000000000, -55.00000000000000000, 220.0000000000000284 ) ) ;
#529 = ADVANCED_FACE ( 'NONE', ( #545, #1858, #8136, #5692, #587, #3655 ), #2328, .F. ) ;
#530 = EDGE_CURVE ( 'NONE', #7082, #2571, #3537, .T. ) ;
#531 = DIRECTION ( 'NONE',  ( 1.000000000000000000, 0.000000000000000000, 0.000000000000000000 ) ) ;
#532 = DIRECTION ( 'NONE',  ( 0.000000000000000000, 0.000000000000000000, -1.000000000000000000 ) ) ;
#533 = CARTESIAN_POINT ( 'NONE',  ( 11.22541203495697104, -48.72469304432832615, -18.06039341770851436 ) ) ;
#534 = CIRCLE ( 'NONE', #1490, 5.000000000000004441 ) ;
#535 = CARTESIAN_POINT ( 'NONE',  ( 0.000000000000000000, 0.000000000000000000, -128.0000000000000284 ) ) ;
#536 = AXIS2_PLACEMENT_3D ( 'NONE', #6714, #5911, #8024 ) ;
#537 = COLOUR_RGB ( '',0.7921568627450980005, 0.8196078431372548767, 0.9333333333333333481 ) ;
#538 = FACE_OUTER_BOUND ( 'NONE', #2255, .T. ) ;
#539 = ORIENTED_EDGE ( 'NONE', *, *, #3641, .F. ) ;
#540 = CIRCLE ( 'NONE', #7016, 5.400000000000035882 ) ;
#541 =( GEOMETRIC_REPRESENTATION_CONTEXT ( 3 ) GLOBAL_UNCERTAINTY_ASSIGNED_CONTEXT ( ( #6320 ) ) GLOBAL_UNIT_ASSIGNED_CONTEXT ( ( #4638, #151, #7345 ) ) REPRESENTATION_CONTEXT ( 'NONE', 'WORKASPACE' ) );
#542 = ORIENTED_EDGE ( 'NONE', *, *, #6069, .T. ) ;
#543 = CARTESIAN_POINT ( 'NONE',  ( 5.551115123125782702E-14, 12.49999999999999645, -1.387778780781445676E-14 ) ) ;
#544 = DIRECTION ( 'NONE',  ( -0.000000000000000000, -0.000000000000000000, 1.000000000000000000 ) ) ;
#545 = FACE_BOUND ( 'NONE', #6221, .T. ) ;
#546 = ORIENTED_EDGE ( 'NONE', *, *, #4676, .T. ) ;
#547 = DIRECTION ( 'NONE',  ( -1.000000000000000000, -0.000000000000000000, -0.000000000000000000 ) ) ;
#548 = CARTESIAN_POINT ( 'NONE',  ( -125.0000000000000000, 125.0000000000000000, -28.00000000000002487 ) ) ;
#549 = VERTEX_POINT ( 'NONE', #6271 ) ;
#550 = SHAPE_DEFINITION_REPRESENTATION ( #6549, #5477 ) ;
#551 = CARTESIAN_POINT ( 'NONE',  ( 12.41819479434714069, 48.43362276422629975, -14.14586790793774895 ) ) ;
#552 = ORIENTED_EDGE ( 'NONE', *, *, #875, .F. ) ;
#553 = DIRECTION ( 'NONE',  ( -0.000000000000000000, -0.000000000000000000, 1.000000000000000000 ) ) ;
#554 = VERTEX_POINT ( 'NONE', #494 ) ;
#555 = CARTESIAN_POINT ( 'NONE',  ( -94.99999999999997158, -95.00000000000008527, 35.00000000000000000 ) ) ;
#556 = CIRCLE ( 'NONE', #6891, 12.99999999999999822 ) ;
#557 = PRODUCT_DEFINITION ( 'UNKNOWN', '', #4198, #6779 ) ;
#558 = CARTESIAN_POINT ( 'NONE',  ( -9.403142016537936243, 49.10855715295182478, -4.253968596005561764 ) ) ;
#559 = ORIENTED_EDGE ( 'NONE', *, *, #4204, .F. ) ;
#560 = ADVANCED_FACE ( 'NONE', ( #3064 ), #3869, .F. ) ;
#561 = EDGE_LOOP ( 'NONE', ( #1225, #8285, #5177, #3711 ) ) ;
#562 = ADVANCED_FACE ( 'NONE', ( #7966 ), #3422, .T. ) ;
#563 = AXIS2_PLACEMENT_3D ( 'NONE', #1559, #5435, #1598 ) ;
#564 = CARTESIAN_POINT ( 'NONE',  ( -60.00000000000000000, 55.00000000000000000, 240.0000000000000284 ) ) ;
#565 = DIRECTION ( 'NONE',  ( -1.000000000000000000, 0.000000000000000000, -0.000000000000000000 ) ) ;
#566 = DIRECTION ( 'NONE',  ( -0.000000000000000000, -0.000000000000000000, 1.000000000000000000 ) ) ;
#567 = ORIENTED_EDGE ( 'NONE', *, *, #3332, .F. ) ;
#568 = DIRECTION ( 'NONE',  ( 1.000000000000000000, 0.000000000000000000, 0.000000000000000000 ) ) ;
#569 = DIRECTION ( 'NONE',  ( 0.000000000000000000, 0.000000000000000000, 1.000000000000000000 ) ) ;
#570 = EDGE_CURVE ( 'NONE', #6321, #3267, #1593, .T. ) ;
#571 = EDGE_LOOP ( 'NONE', ( #8103, #3538 ) ) ;
#572 = CARTESIAN_POINT ( 'NONE',  ( 0.000000000000000000, 0.000000000000000000, 57.99999999999999289 ) ) ;
#573 = SHAPE_REPRESENTATION ( 'Probe', ( #1299 ), #7094 ) ;
#574 = CARTESIAN_POINT ( 'NONE',  ( -105.9999999999999858, -114.9999999999999858, 20.00000000000000000 ) ) ;
#575 = CARTESIAN_POINT ( 'NONE',  ( 9.403142016537936243, -49.10855715295183188, -4.253968596005562652 ) ) ;
#576 = FACE_OUTER_BOUND ( 'NONE', #5063, .T. ) ;
#577 = AXIS2_PLACEMENT_3D ( 'NONE', #4578, #1221, #3947 ) ;
#578 = FACE_OUTER_BOUND ( 'NONE', #61, .T. ) ;
#579 = ADVANCED_FACE ( 'NONE', ( #2155 ), #2747, .F. ) ;
#580 = ORIENTED_EDGE ( 'NONE', *, *, #3848, .T. ) ;
#581 = EDGE_CURVE ( 'NONE', #7933, #4405, #6106, .T. ) ;
#582 = DIRECTION ( 'NONE',  ( 0.7071067811865487940, 0.000000000000000000, -0.7071067811865463515 ) ) ;
#583 = AXIS2_PLACEMENT_3D ( 'NONE', #4746, #5934, #7328 ) ;
#584 = UNCERTAINTY_MEASURE_WITH_UNIT (LENGTH_MEASURE( 1.000000000000000082E-05 ), #5485, 'distance_accuracy_value', 'NONE');
#585 = ORIENTED_EDGE ( 'NONE', *, *, #8135, .F. ) ;
#586 = LINE ( 'NONE', #6396, #3892 ) ;
#587 = FACE_OUTER_BOUND ( 'NONE', #4365, .T. ) ;
#588 = EDGE_LOOP ( 'NONE', ( #4360, #4935, #2316, #3157, #5452 ) ) ;
#589 = LINE ( 'NONE', #629, #1204 ) ;
#590 = DIRECTION ( 'NONE',  ( -0.000000000000000000, -0.000000000000000000, -1.000000000000000000 ) ) ;
#591 = ORIENTED_EDGE ( 'NONE', *, *, #4122, .F. ) ;
#592 = CARTESIAN_POINT ( 'NONE',  ( 4.037232620646171277, 49.84250566375262537, -24.35825330067164884 ) ) ;
#593 = EDGE_LOOP ( 'NONE', ( #552, #7812 ) ) ;
#594 = ADVANCED_BREP_SHAPE_REPRESENTATION ( '', ( #3512, #1299 ), #2770 ) ;
#595 = DIRECTION ( 'NONE',  ( 0.000000000000000000, 1.000000000000000000, 0.000000000000000000 ) ) ;
#596 = ORIENTED_EDGE ( 'NONE', *, *, #2034, .T. ) ;
#597 = CARTESIAN_POINT ( 'NONE',  ( 5.000000000000000000, -2.342598717236909600, -4.057499999999997442 ) ) ;
#598 = AXIS2_PLACEMENT_3D ( 'NONE', #1970, #37, #7220 ) ;
#599 = ORIENTED_EDGE ( 'NONE', *, *, #1346, .F. ) ;
#600 = CARTESIAN_POINT ( 'NONE',  ( -31.74999999999995737, 6.123233995736809670E-16, -5.000000000000035527 ) ) ;
#601 = ORIENTED_EDGE ( 'NONE', *, *, #7179, .F. ) ;
#602 = CARTESIAN_POINT ( 'NONE',  ( 0.000000000000000000, 0.000000000000000000, 20.00000000000000355 ) ) ;
#603 = LINE ( 'NONE', #4471, #650 ) ;
#604 = DIRECTION ( 'NONE',  ( -1.000000000000000000, 0.000000000000000000, 0.000000000000000000 ) ) ;
#605 = DIRECTION ( 'NONE',  ( 1.000000000000000000, 0.000000000000000000, 0.000000000000000000 ) ) ;
#606 = ADVANCED_FACE ( 'NONE', ( #7629 ), #2357, .F. ) ;
#607 = CIRCLE ( 'NONE', #7489, 5.999999999999991118 ) ;
#608 = EDGE_LOOP ( 'NONE', ( #5995, #599, #5529 ) ) ;
#609 = PRESENTATION_STYLE_ASSIGNMENT (( #8336 ) ) ;
#610 = ADVANCED_FACE ( 'NONE', ( #5041 ), #4306, .T. ) ;
#611 = DIRECTION ( 'NONE',  ( 0.000000000000000000, 0.000000000000000000, 1.000000000000000000 ) ) ;
#612 = EDGE_LOOP ( 'NONE', ( #6446, #1124, #2582, #4474, #7041 ) ) ;
#613 = CARTESIAN_POINT ( 'NONE',  ( 0.000000000000000000, 0.000000000000000000, 35.00000000000000000 ) ) ;
#614 = DIRECTION ( 'NONE',  ( 1.000000000000000000, 0.000000000000000000, 0.000000000000000000 ) ) ;
#615 = EDGE_CURVE ( 'NONE', #4158, #3739, #1807, .T. ) ;
#616 = DIRECTION ( 'NONE',  ( -0.000000000000000000, -0.000000000000000000, 1.000000000000000000 ) ) ;
#617 = ADVANCED_FACE ( 'NONE', ( #5555 ), #6947, .T. ) ;
#618 = CARTESIAN_POINT ( 'NONE',  ( 12.39753912377990552, -48.43864980223353456, -14.14916085730400219 ) ) ;
#619 = EDGE_CURVE ( 'NONE', #372, #3698, #5183, .T. ) ;
#620 = DIRECTION ( 'NONE',  ( 1.000000000000000000, -0.000000000000000000, 0.000000000000000000 ) ) ;
#621 = LINE ( 'NONE', #7198, #5046 ) ;
#622 = DIRECTION ( 'NONE',  ( -1.000000000000000000, 0.000000000000000000, -0.000000000000000000 ) ) ;
#623 = ORIENTED_EDGE ( 'NONE', *, *, #2527, .F. ) ;
#624 = VERTEX_POINT ( 'NONE', #5765 ) ;
#625 = EDGE_LOOP ( 'NONE', ( #5499, #7571, #8014, #125 ) ) ;
#626 = DIRECTION ( 'NONE',  ( 0.000000000000000000, 0.000000000000000000, -1.000000000000000000 ) ) ;
#627 = AXIS2_PLACEMENT_3D ( 'NONE', #6959, #2577, #1183 ) ;
#628 = ORIENTED_EDGE ( 'NONE', *, *, #6965, .T. ) ;
#629 = CARTESIAN_POINT ( 'NONE',  ( -120.0000000000000000, -125.0000000000000000, -28.00000000000002487 ) ) ;
#630 = CARTESIAN_POINT ( 'NONE',  ( -105.0000000000000000, -72.49999999999994316, 20.00000000000002842 ) ) ;
#631 = ORIENTED_EDGE ( 'NONE', *, *, #7077, .T. ) ;
#632 = DIRECTION ( 'NONE',  ( 0.000000000000000000, -1.000000000000000000, 1.266875999117951024E-16 ) ) ;
#633 = VECTOR ( 'NONE', #208, 1000.000000000000000 ) ;
#634 = ORIENTED_EDGE ( 'NONE', *, *, #7886, .T. ) ;
#635 = DIRECTION ( 'NONE',  ( -0.000000000000000000, -0.000000000000000000, -1.000000000000000000 ) ) ;
#636 = ORIENTED_EDGE ( 'NONE', *, *, #7056, .T. ) ;
#637 = ORIENTED_EDGE ( 'NONE', *, *, #6590, .T. ) ;
#638 = FILL_AREA_STYLE_COLOUR ( '', #8211 ) ;
#639 = AXIS2_PLACEMENT_3D ( 'NONE', #5635, #1167, #8220 ) ;
#640 = DIRECTION ( 'NONE',  ( 0.000000000000000000, -7.945337353457666666E-18, -1.000000000000000000 ) ) ;
#641 = ORIENTED_EDGE ( 'NONE', *, *, #6036, .F. ) ;
#642 = AXIS2_PLACEMENT_3D ( 'NONE', #2714, #6722, #256 ) ;
#643 = LINE ( 'NONE', #4722, #6660 ) ;
#644 = LINE ( 'NONE', #2550, #3740 ) ;
#645 = CARTESIAN_POINT ( 'NONE',  ( 114.9999999999999147, 115.0000000000000000, 250.0000000000000000 ) ) ;
#646 = AXIS2_PLACEMENT_3D ( 'NONE', #788, #6612, #832 ) ;
#647 = LINE ( 'NONE', #3893, #4845 ) ;
#648 = ORIENTED_EDGE ( 'NONE', *, *, #3135, .T. ) ;
#649 = LINE ( 'NONE', #1933, #4243 ) ;
#650 = VECTOR ( 'NONE', #7306, 1000.000000000000000 ) ;
#651 = ORIENTED_EDGE ( 'NONE', *, *, #7751, .F. ) ;
#652 = AXIS2_PLACEMENT_3D ( 'NONE', #316, #3056, #8044 ) ;
#653 = VERTEX_POINT ( 'NONE', #4478 ) ;
#654 = ADVANCED_FACE ( 'NONE', ( #5169 ), #7069, .F. ) ;
#655 = CYLINDRICAL_SURFACE ( 'NONE', #1454, 75.00000000000001421 ) ;
#656 = AXIS2_PLACEMENT_3D ( 'NONE', #8184, #408, #2979 ) ;
#657 = PLANE ( 'NONE',  #5711 ) ;
#658 = CARTESIAN_POINT ( 'NONE',  ( 10.16267929626374489, -48.95685099404312979, -19.78936650929338725 ) ) ;
#659 = DIRECTION ( 'NONE',  ( -1.000000000000000000, 0.000000000000000000, 0.000000000000000000 ) ) ;
#660 = VECTOR ( 'NONE', #5010, 1000.000000000000000 ) ;
#661 = FACE_OUTER_BOUND ( 'NONE', #6204, .T. ) ;
#662 = ORIENTED_EDGE ( 'NONE', *, *, #737, .F. ) ;
#663 = DIRECTION ( 'NONE',  ( 1.000000000000000000, 0.000000000000000000, 0.000000000000000000 ) ) ;
#664 = EDGE_CURVE ( 'NONE', #8205, #351, #3409, .T. ) ;
#665 = ADVANCED_FACE ( 'NONE', ( #7284 ), #4016, .F. ) ;
#666 = ADVANCED_FACE ( 'NONE', ( #5376 ), #6607, .T. ) ;
#667 = ORIENTED_EDGE ( 'NONE', *, *, #3851, .F. ) ;
#668 = ORIENTED_EDGE ( 'NONE', *, *, #4872, .F. ) ;
#669 = CARTESIAN_POINT ( 'NONE',  ( 120.5000000000000000, 114.9999999999999716, 10.00000000000000000 ) ) ;
#670 = VECTOR ( 'NONE', #4828, 1000.000000000000000 ) ;
#671 = CIRCLE ( 'NONE', #3474, 57.99999999999995737 ) ;
#672 = EDGE_LOOP ( 'NONE', ( #3276, #4594, #7730, #8070 ) ) ;
#673 = CARTESIAN_POINT ( 'NONE',  ( 115.0000000000000284, -115.0000000000000000, 20.00000000000000355 ) ) ;
#674 = FACE_OUTER_BOUND ( 'NONE', #5673, .T. ) ;
#675 = DIRECTION ( 'NONE',  ( 0.000000000000000000, -1.000000000000000000, 0.000000000000000000 ) ) ;
#676 = CONTEXT_DEPENDENT_SHAPE_REPRESENTATION ( #8123, #3921 ) ;
#677 = DIRECTION ( 'NONE',  ( 1.000000000000000000, 0.000000000000000000, 0.000000000000000000 ) ) ;
#678 = ORIENTED_EDGE ( 'NONE', *, *, #2723, .T. ) ;
#679 = VECTOR ( 'NONE', #7829, 1000.000000000000000 ) ;
#680 = EDGE_CURVE ( 'NONE', #1656, #1706, #2751, .T. ) ;
#681 = CARTESIAN_POINT ( 'NONE',  ( 95.00000000000000000, 95.00000000000008527, 35.00000000000000000 ) ) ;
#682 = LINE ( 'NONE', #2005, #3999 ) ;
#683 = EDGE_LOOP ( 'NONE', ( #5430, #349 ) ) ;
#684 = PRESENTATION_STYLE_ASSIGNMENT (( #1314 ) ) ;
#685 = VECTOR ( 'NONE', #498, 1000.000000000000000 ) ;
#686 = CARTESIAN_POINT ( 'NONE',  ( -120.4999999999999858, -114.9999999999999858, 0.000000000000000000 ) ) ;
#687 = ORIENTED_EDGE ( 'NONE', *, *, #3635, .T. ) ;
#688 = EDGE_CURVE ( 'NONE', #7860, #57, #8154, .T. ) ;
#689 = FACE_BOUND ( 'NONE', #7167, .T. ) ;
#690 = CARTESIAN_POINT ( 'NONE',  ( 0.000000000000000000, 72.49999999999995737, 79.99999999999994316 ) ) ;
#691 = LINE ( 'NONE', #8174, #113 ) ;
#692 = PRODUCT_DEFINITION_SHAPE ( 'NONE', 'NONE',  #8367 ) ;
#693 = FACE_OUTER_BOUND ( 'NONE', #2495, .T. ) ;
#694 = ORIENTED_EDGE ( 'NONE', *, *, #5974, .T. ) ;
#695 = LINE ( 'NONE', #5367, #1574 ) ;
#696 = DIRECTION ( 'NONE',  ( 0.000000000000000000, 0.000000000000000000, 1.000000000000000000 ) ) ;
#697 = ORIENTED_EDGE ( 'NONE', *, *, #8210, .F. ) ;
#698 = VERTEX_POINT ( 'NONE', #4611 ) ;
#699 = CARTESIAN_POINT ( 'NONE',  ( -55.00000000000000000, -55.00000000000000000, 220.0000000000000284 ) ) ;
#700 = CIRCLE ( 'NONE', #5822, 5.000000000000070166 ) ;
#701 = CARTESIAN_POINT ( 'NONE',  ( -60.00000000000000000, -55.00000000000000000, 240.0000000000000284 ) ) ;
#702 = CARTESIAN_POINT ( 'NONE',  ( 6.614448519079572542, -49.56174273647120998, -23.11440585317444985 ) ) ;
#703 = LINE ( 'NONE', #5265, #4111 ) ;
#704 = DIRECTION ( 'NONE',  ( -0.000000000000000000, -0.000000000000000000, -1.000000000000000000 ) ) ;
#705 = EDGE_LOOP ( 'NONE', ( #4300, #4268, #4984, #5088 ) ) ;
#706 = MANIFOLD_SOLID_BREP ( 'Cut-Extrude1', #310 ) ;
#707 = EDGE_LOOP ( 'NONE', ( #6265, #1176, #18, #8160, #1408, #795, #3196, #6738 ) ) ;
#708 = ORIENTED_EDGE ( 'NONE', *, *, #4152, .F. ) ;
#709 = CARTESIAN_POINT ( 'NONE',  ( 0.000000000000000000, 0.000000000000000000, 35.00000000000000000 ) ) ;
#710 = PRODUCT_RELATED_PRODUCT_CATEGORY ( 'part', '', ( #7957 ) ) ;
#711 = ORIENTED_EDGE ( 'NONE', *, *, #3187, .T. ) ;
#712 = DIRECTION ( 'NONE',  ( 1.000000000000000000, 0.000000000000000000, 0.000000000000000000 ) ) ;
#713 = AXIS2_PLACEMENT_3D ( 'NONE', #6201, #3523, #6104 ) ;
#714 = DIRECTION ( 'NONE',  ( -1.752490724247359037E-17, 1.000000000000000000, 3.853078496550133260E-17 ) ) ;
#715 = EDGE_CURVE ( 'NONE', #3072, #2500, #2204, .T. ) ;
#716 = CARTESIAN_POINT ( 'NONE',  ( 106.0000000000000142, -114.9999999999999716, 20.00000000000000000 ) ) ;
#717 = VERTEX_POINT ( 'NONE', #5434 ) ;
#718 = VERTEX_POINT ( 'NONE', #4108 ) ;
#719 = VECTOR ( 'NONE', #8002, 1000.000000000000000 ) ;
#720 = CARTESIAN_POINT ( 'NONE',  ( 17.61817604250836311, 0.000000000000000000, -118.0000000000000284 ) ) ;
#721 = EDGE_CURVE ( 'NONE', #7126, #7967, #3963, .T. ) ;
#722 = CARTESIAN_POINT ( 'NONE',  ( 5.551115123125782702E-14, 12.50000000000001066, -1.387778780781445676E-14 ) ) ;
#723 = ORIENTED_EDGE ( 'NONE', *, *, #8302, .T. ) ;
#724 = DIRECTION ( 'NONE',  ( 0.000000000000000000, 0.000000000000000000, -1.000000000000000000 ) ) ;
#725 = ADVANCED_FACE ( 'NONE', ( #4875 ), #7426, .F. ) ;
#726 = CARTESIAN_POINT ( 'NONE',  ( 59.99999999999999289, 55.00000000000000000, 220.0000000000000284 ) ) ;
#727 = CARTESIAN_POINT ( 'NONE',  ( 10.00000000000000000, 57.99999999999990052, 93.75000000000004263 ) ) ;
#728 = DIRECTION ( 'NONE',  ( 0.000000000000000000, 0.000000000000000000, 1.000000000000000000 ) ) ;
#729 = CLOSED_SHELL ( 'NONE', ( #3816, #7770, #7786, #6914, #1126, #1756 ) ) ;
#730 = DIRECTION ( 'NONE',  ( -0.000000000000000000, 1.000000000000000000, 1.224646799147353207E-16 ) ) ;
#731 = LINE ( 'NONE', #7181, #4203 ) ;
#732 = LINE ( 'NONE', #8263, #8074 ) ;
#733 = DIRECTION ( 'NONE',  ( 0.000000000000000000, 0.000000000000000000, -1.000000000000000000 ) ) ;
#734 = EDGE_LOOP ( 'NONE', ( #5853, #4869 ) ) ;
#735 = EDGE_CURVE ( 'NONE', #3015, #3602, #6056, .T. ) ;
#736 = CARTESIAN_POINT ( 'NONE',  ( 55.00000000000000000, 55.00000000000000000, 220.0000000000000284 ) ) ;
#737 = EDGE_CURVE ( 'NONE', #986, #5147, #4224, .T. ) ;
#738 = VECTOR ( 'NONE', #3922, 1000.000000000000000 ) ;
#739 = ORIENTED_EDGE ( 'NONE', *, *, #1590, .T. ) ;
#740 = EDGE_CURVE ( 'NONE', #2575, #6246, #8045, .T. ) ;
#741 = LINE ( 'NONE', #2603, #1864 ) ;
#742 = VECTOR ( 'NONE', #864, 1000.000000000000000 ) ;
#743 = FACE_OUTER_BOUND ( 'NONE', #5654, .T. ) ;
#744 = LINE ( 'NONE', #906, #4238 ) ;
#745 = CIRCLE ( 'NONE', #1834, 4.057500000000000107 ) ;
#746 = FACE_OUTER_BOUND ( 'NONE', #7315, .T. ) ;
#747 = EDGE_LOOP ( 'NONE', ( #539, #13, #8100 ) ) ;
#748 = ORIENTED_EDGE ( 'NONE', *, *, #2964, .F. ) ;
#749 = FACE_OUTER_BOUND ( 'NONE', #4846, .T. ) ;
#750 = ORIENTED_EDGE ( 'NONE', *, *, #3807, .F. ) ;
#751 = CARTESIAN_POINT ( 'NONE',  ( -15.00000000000000000, 1.836970198721029589E-15, -128.0000000000000284 ) ) ;
#752 = CARTESIAN_POINT ( 'NONE',  ( -54.99999999999999289, 75.00000000000000000, 27.50000000000000000 ) ) ;
#753 = AXIS2_PLACEMENT_3D ( 'NONE', #5334, #785, #7918 ) ;
#754 = DIRECTION ( 'NONE',  ( 1.000000000000000000, 0.000000000000000000, 0.000000000000000000 ) ) ;
#755 = EDGE_LOOP ( 'NONE', ( #6173, #4215, #4913, #5960 ) ) ;
#756 = PRODUCT_DEFINITION_SHAPE ( 'NONE', 'NONE',  #8363 ) ;
#757 = ADVANCED_FACE ( 'NONE', ( #3388 ), #6254, .T. ) ;
#758 = VERTEX_POINT ( 'NONE', #317 ) ;
#759 = DIRECTION ( 'NONE',  ( -0.000000000000000000, -0.000000000000000000, 1.000000000000000000 ) ) ;
#760 = ORIENTED_EDGE ( 'NONE', *, *, #7716, .F. ) ;
#761 = CARTESIAN_POINT ( 'NONE',  ( -121.0000000000000284, -115.0000000000000000, 70.00000000000000000 ) ) ;
#762 = DIRECTION ( 'NONE',  ( -1.000000000000000000, -0.000000000000000000, -0.000000000000000000 ) ) ;
#763 = DIRECTION ( 'NONE',  ( -1.000000000000000000, 0.000000000000000000, 0.000000000000000000 ) ) ;
#764 = EDGE_LOOP ( 'NONE', ( #7104, #4270, #4312, #1914 ) ) ;
#765 = CIRCLE ( 'NONE', #5482, 5.999999999999991118 ) ;
#766 = LINE ( 'NONE', #1, #7092 ) ;
#767 = EDGE_CURVE ( 'NONE', #3292, #4329, #8159, .T. ) ;
#768 = DIRECTION ( 'NONE',  ( 1.000000000000000000, 0.000000000000000000, 0.000000000000000000 ) ) ;
#769 = ADVANCED_FACE ( 'NONE', ( #2765 ), #1004, .T. ) ;
#770 = DIRECTION ( 'NONE',  ( -0.8571673007021112234, 1.049727191138617340E-16, 0.5150380749100560429 ) ) ;
#771 = CARTESIAN_POINT ( 'NONE',  ( 75.00000000000001421, 9.184850993605150311E-15, 57.99999999999999289 ) ) ;
#772 = AXIS2_PLACEMENT_3D ( 'NONE', #5605, #2410, #3654 ) ;
#773 = CYLINDRICAL_SURFACE ( 'NONE', #4839, 5.999999999999991118 ) ;
#774 = DIRECTION ( 'NONE',  ( 1.000000000000000000, 0.000000000000000000, 0.000000000000000000 ) ) ;
#775 = ORIENTED_EDGE ( 'NONE', *, *, #5713, .F. ) ;
#776 = PLANE ( 'NONE',  #6139 ) ;
#777 = DIRECTION ( 'NONE',  ( 1.224646799147346798E-16, 3.155443620884047222E-30, -1.000000000000000000 ) ) ;
#778 = ORIENTED_EDGE ( 'NONE', *, *, #5207, .F. ) ;
#779 = AXIS2_PLACEMENT_3D ( 'NONE', #7723, #2681, #5258 ) ;
#780 = CIRCLE ( 'NONE', #5493, 5.499999999999991118 ) ;
#781 = DIRECTION ( 'NONE',  ( -0.000000000000000000, -7.945337353457666666E-18, -1.000000000000000000 ) ) ;
#782 = DIRECTION ( 'NONE',  ( -0.000000000000000000, -0.000000000000000000, 1.000000000000000000 ) ) ;
#783 = VECTOR ( 'NONE', #770, 1000.000000000000000 ) ;
#784 = LINE ( 'NONE', #7845, #3091 ) ;
#785 = DIRECTION ( 'NONE',  ( 0.000000000000000000, 0.000000000000000000, 1.000000000000000000 ) ) ;
#786 = CARTESIAN_POINT ( 'NONE',  ( 114.9999999999999147, 115.0000000000000000, 8.205133554287239938E-16 ) ) ;
#787 = CIRCLE ( 'NONE', #5776, 4.999999999999997335 ) ;
#788 = CARTESIAN_POINT ( 'NONE',  ( -125.0000000000000000, -125.0000000000000284, 70.00000000000000000 ) ) ;
#789 = ORIENTED_EDGE ( 'NONE', *, *, #1988, .T. ) ;
#790 = VECTOR ( 'NONE', #7088, 1000.000000000000000 ) ;
#791 = DIRECTION ( 'NONE',  ( 0.000000000000000000, 1.000000000000000000, -7.945337353457666666E-18 ) ) ;
#792 = EDGE_CURVE ( 'NONE', #5384, #549, #5347, .T. ) ;
#793 = VECTOR ( 'NONE', #4334, 1000.000000000000000 ) ;
#794 = DIRECTION ( 'NONE',  ( -0.000000000000000000, -0.000000000000000000, 1.000000000000000000 ) ) ;
#795 = ORIENTED_EDGE ( 'NONE', *, *, #6434, .F. ) ;
#796 = ORIENTED_EDGE ( 'NONE', *, *, #4247, .F. ) ;
#797 = DIRECTION ( 'NONE',  ( 1.000000000000000000, 0.000000000000000000, 0.000000000000000000 ) ) ;
#798 = FACE_BOUND ( 'NONE', #2089, .T. ) ;
#799 = AXIS2_PLACEMENT_3D ( 'NONE', #2892, #1645, #6922 ) ;
#800 = CIRCLE ( 'NONE', #7265, 5.000000000000035527 ) ;
#801 = FACE_OUTER_BOUND ( 'NONE', #4380, .T. ) ;
#802 = CIRCLE ( 'NONE', #2559, 15.00000000000000178 ) ;
#803 = VECTOR ( 'NONE', #819, 1000.000000000000000 ) ;
#804 = CARTESIAN_POINT ( 'NONE',  ( -115.0000000000000000, 115.0000000000000000, 340.0000000000000000 ) ) ;
#805 = VERTEX_POINT ( 'NONE', #4712 ) ;
#806 = FILL_AREA_STYLE ('',( #2168 ) ) ;
#807 = CONICAL_SURFACE ( 'NONE', #951, 12.50000000000000000, 0.7853981633974560506 ) ;
#808 = AXIS2_PLACEMENT_3D ( 'NONE', #888, #4718, #2129 ) ;
#809 = ORIENTED_EDGE ( 'NONE', *, *, #1189, .T. ) ;
#810 = DIRECTION ( 'NONE',  ( 0.000000000000000000, -1.000000000000000000, -1.632680918566406547E-16 ) ) ;
#811 = CARTESIAN_POINT ( 'NONE',  ( -115.0000000000000000, 115.0000000000000000, 70.00000000000000000 ) ) ;
#812 = ORIENTED_EDGE ( 'NONE', *, *, #1185, .F. ) ;
#813 = PRODUCT_DEFINITION_SHAPE ( 'NONE', 'NONE',  #2910 ) ;
#814 = CARTESIAN_POINT ( 'NONE',  ( 106.0000000000000142, 114.9999999999999716, 20.00000000000000000 ) ) ;
#815 = DIRECTION ( 'NONE',  ( -0.000000000000000000, -1.460819769243626884E-16, 1.000000000000000000 ) ) ;
#816 = CIRCLE ( 'NONE', #7702, 4.999999999999990230 ) ;
#817 = DIRECTION ( 'NONE',  ( 0.000000000000000000, 0.000000000000000000, -1.000000000000000000 ) ) ;
#818 = DIRECTION ( 'NONE',  ( 1.000000000000000000, -9.992007221626408864E-16, 0.000000000000000000 ) ) ;
#819 = DIRECTION ( 'NONE',  ( 0.000000000000000000, -2.960594732333750117E-16, 1.000000000000000000 ) ) ;
#820 = PRODUCT_RELATED_PRODUCT_CATEGORY ( 'part', '', ( #4297 ) ) ;
#821 = DIRECTION ( 'NONE',  ( 1.000000000000000000, 0.000000000000000000, 0.000000000000000000 ) ) ;
#822 = ORIENTED_EDGE ( 'NONE', *, *, #4122, .T. ) ;
#823 = CARTESIAN_POINT ( 'NONE',  ( 0.000000000000000000, 0.000000000000000000, -128.0000000000000284 ) ) ;
#824 = ADVANCED_FACE ( 'NONE', ( #6135 ), #881, .F. ) ;
#825 = ORIENTED_EDGE ( 'NONE', *, *, #335, .F. ) ;
#826 = MANIFOLD_SOLID_BREP ( 'CBORE for M10 SHCS1', #2352 ) ;
#827 = CARTESIAN_POINT ( 'NONE',  ( -15.00000000000000000, 1.836970198721029589E-15, -126.0000000000000284 ) ) ;
#828 = CARTESIAN_POINT ( 'NONE',  ( 75.00000000000000000, 55.00000000000000711, -27.50000000000000000 ) ) ;
#829 = PRESENTATION_STYLE_ASSIGNMENT (( #7237 ) ) ;
#830 = EDGE_CURVE ( 'NONE', #718, #2876, #7035, .T. ) ;
#831 = DIRECTION ( 'NONE',  ( 1.000000000000000000, 0.000000000000000000, 0.000000000000000000 ) ) ;
#832 = DIRECTION ( 'NONE',  ( 0.000000000000000000, 0.000000000000000000, -1.000000000000000000 ) ) ;
#833 = ORIENTED_EDGE ( 'NONE', *, *, #6845, .F. ) ;
#834 = AXIS2_PLACEMENT_3D ( 'NONE', #2619, #5348, #2002 ) ;
#835 = CARTESIAN_POINT ( 'NONE',  ( -1.173433385984103696E-13, -12.50000000000001066, -12.49999999999998757 ) ) ;
#836 = VERTEX_POINT ( 'NONE', #6820 ) ;
#837 = EDGE_LOOP ( 'NONE', ( #1271, #3506, #2194, #809 ) ) ;
#838 = CARTESIAN_POINT ( 'NONE',  ( 0.000000000000000000, 4.500000000000000000, -126.0000000000000284 ) ) ;
#839 = LINE ( 'NONE', #6529, #4130 ) ;
#840 = EDGE_CURVE ( 'NONE', #4413, #3125, #621, .T. ) ;
#841 = ORIENTED_EDGE ( 'NONE', *, *, #8140, .T. ) ;
#842 = CIRCLE ( 'NONE', #983, 4.999999999999990230 ) ;
#843 = EDGE_LOOP ( 'NONE', ( #1832, #4978 ) ) ;
#844 = CARTESIAN_POINT ( 'NONE',  ( -114.9999999999999716, 114.9999999999999858, 0.000000000000000000 ) ) ;
#845 = ORIENTED_EDGE ( 'NONE', *, *, #5575, .F. ) ;
#846 = FACE_OUTER_BOUND ( 'NONE', #1424, .T. ) ;
#847 = DIRECTION ( 'NONE',  ( 0.000000000000000000, 0.000000000000000000, 1.000000000000000000 ) ) ;
#848 = CIRCLE ( 'NONE', #1394, 5.999999999999991118 ) ;
#849 = AXIS2_PLACEMENT_3D ( 'NONE', #2893, #2068, #6101 ) ;
#850 = DIRECTION ( 'NONE',  ( -0.000000000000000000, -0.000000000000000000, 1.000000000000000000 ) ) ;
#851 = CARTESIAN_POINT ( 'NONE',  ( 125.0000000000000000, -125.0000000000000000, 340.0000000000000000 ) ) ;
#852 = DIRECTION ( 'NONE',  ( 1.000000000000000000, 0.000000000000000000, 0.000000000000000000 ) ) ;
#853 = CARTESIAN_POINT ( 'NONE',  ( 115.0000000000000000, -114.9999999999999716, 10.00000000000000000 ) ) ;
#854 = VECTOR ( 'NONE', #4682, 1000.000000000000000 ) ;
#855 = CARTESIAN_POINT ( 'NONE',  ( -10.00000000000000000, 57.99999999999997868, -93.74999999999997158 ) ) ;
#856 = ORIENTED_EDGE ( 'NONE', *, *, #2130, .F. ) ;
#857 = CARTESIAN_POINT ( 'NONE',  ( 17.61817604250836311, 0.000000000000000000, -126.0000000000000284 ) ) ;
#858 = AXIS2_PLACEMENT_3D ( 'NONE', #1793, #3675, #1748 ) ;
#859 = EDGE_LOOP ( 'NONE', ( #1022, #5933, #4897, #7019 ) ) ;
#860 = VERTEX_POINT ( 'NONE', #1420 ) ;
#861 = DIRECTION ( 'NONE',  ( 0.000000000000000000, 0.000000000000000000, -1.000000000000000000 ) ) ;
#862 = ADVANCED_FACE ( 'NONE', ( #7728 ), #3981, .F. ) ;
#863 = EDGE_CURVE ( 'NONE', #7276, #4717, #4483, .T. ) ;
#864 = DIRECTION ( 'NONE',  ( -0.000000000000000000, -7.945337353457666666E-18, -1.000000000000000000 ) ) ;
#865 = CARTESIAN_POINT ( 'NONE',  ( -125.0000000000000000, 125.0000000000000284, 70.00000000000000000 ) ) ;
#866 = CIRCLE ( 'NONE', #4079, 57.99999999999995737 ) ;
#867 = CARTESIAN_POINT ( 'NONE',  ( 125.0000000000000000, -125.0000000000000284, 70.00000000000000000 ) ) ;
#868 = LINE ( 'NONE', #4741, #4236 ) ;
#869 = DIRECTION ( 'NONE',  ( 1.000000000000000000, 0.000000000000000000, 0.000000000000000000 ) ) ;
#870 = ORIENTED_EDGE ( 'NONE', *, *, #4995, .T. ) ;
#871 = EDGE_CURVE ( 'NONE', #1109, #6237, #1148, .T. ) ;
#872 = DIRECTION ( 'NONE',  ( -1.000000000000000000, 0.000000000000000000, 0.000000000000000000 ) ) ;
#873 = AXIS2_PLACEMENT_3D ( 'NONE', #2320, #8006, #5392 ) ;
#874 = ADVANCED_FACE ( 'NONE', ( #1584 ), #2839, .F. ) ;
#875 = EDGE_CURVE ( 'NONE', #5541, #902, #607, .T. ) ;
#876 = DIRECTION ( 'NONE',  ( -0.000000000000000000, -1.460819769243626884E-16, 1.000000000000000000 ) ) ;
#877 = VERTEX_POINT ( 'NONE', #3456 ) ;
#878 = DIRECTION ( 'NONE',  ( 1.000000000000000000, 0.000000000000000000, -0.000000000000000000 ) ) ;
#879 = CARTESIAN_POINT ( 'NONE',  ( 115.0000000000000000, 115.0000000000000000, 270.0000000000000000 ) ) ;
#880 = PRESENTATION_LAYER_ASSIGNMENT (  '', '', ( #2111 ) ) ;
#881 = CYLINDRICAL_SURFACE ( 'NONE', #5727, 95.00000000000008527 ) ;
#882 = DIRECTION ( 'NONE',  ( -1.000000000000000000, -0.000000000000000000, -0.000000000000000000 ) ) ;
#883 = ORIENTED_EDGE ( 'NONE', *, *, #2186, .T. ) ;
#884 = ORIENTED_EDGE ( 'NONE', *, *, #4049, .F. ) ;
#885 = EDGE_CURVE ( 'NONE', #1626, #6639, #3839, .T. ) ;
#886 = DIRECTION ( 'NONE',  ( -0.000000000000000000, -0.000000000000000000, 1.000000000000000000 ) ) ;
#887 = ORIENTED_EDGE ( 'NONE', *, *, #4997, .T. ) ;
#888 = CARTESIAN_POINT ( 'NONE',  ( -54.99999999999999289, -55.00000000000000711, 27.50000000000000000 ) ) ;
#889 = CARTESIAN_POINT ( 'NONE',  ( 0.000000000000000000, -72.49999999999998579, 66.99999999999995737 ) ) ;
#890 = PLANE ( 'NONE',  #4820 ) ;
#891 = ADVANCED_BREP_SHAPE_REPRESENTATION ( '', ( #826, #1299 ), #3387 ) ;
#892 = ADVANCED_FACE ( 'NONE', ( #5421 ), #4138, .F. ) ;
#893 = FACE_BOUND ( 'NONE', #1076, .T. ) ;
#894 = DIRECTION ( 'NONE',  ( 0.000000000000000000, -0.000000000000000000, -1.000000000000000000 ) ) ;
#895 = LINE ( 'NONE', #5989, #5171 ) ;
#896 = DIRECTION ( 'NONE',  ( 1.000000000000000000, 0.000000000000000000, 0.000000000000000000 ) ) ;
#897 = CIRCLE ( 'NONE', #5065, 15.00000000000000000 ) ;
#898 = LINE ( 'NONE', #5411, #1902 ) ;
#899 = ORIENTED_EDGE ( 'NONE', *, *, #2632, .F. ) ;
#900 = VERTEX_POINT ( 'NONE', #1546 ) ;
#901 = CIRCLE ( 'NONE', #2392, 5.999999999999991118 ) ;
#902 = VERTEX_POINT ( 'NONE', #2874 ) ;
#903 = FACE_OUTER_BOUND ( 'NONE', #8243, .T. ) ;
#904 = CARTESIAN_POINT ( 'NONE',  ( 121.0000000000000284, -115.0000000000000000, 20.00000000000000355 ) ) ;
#905 = CARTESIAN_POINT ( 'NONE',  ( 0.000000000000000000, -5.000000000000000000, 57.99999999999999289 ) ) ;
#906 = CARTESIAN_POINT ( 'NONE',  ( -0.000000000000000000, -115.0000000000000000, 0.000000000000000000 ) ) ;
#907 = VECTOR ( 'NONE', #3781, 1000.000000000000000 ) ;
#908 = CARTESIAN_POINT ( 'NONE',  ( 6.123233995736765296E-15, -49.99999999999999289, -250.0000000000000000 ) ) ;
#909 = ORIENTED_EDGE ( 'NONE', *, *, #2279, .F. ) ;
#910 = FACE_OUTER_BOUND ( 'NONE', #7824, .T. ) ;
#911 = VECTOR ( 'NONE', #1701, 1000.000000000000000 ) ;
#912 = CARTESIAN_POINT ( 'NONE',  ( -54.99999999999999289, 55.00000000000000711, -27.50000000000000000 ) ) ;
#913 = CIRCLE ( 'NONE', #5356, 15.00000000000000000 ) ;
#914 = ORIENTED_EDGE ( 'NONE', *, *, #3174, .T. ) ;
#915 = CARTESIAN_POINT ( 'NONE',  ( -105.0000000000000000, 8.487013464091010249E-14, 20.00000000000001776 ) ) ;
#916 = CARTESIAN_POINT ( 'NONE',  ( 10.00000000000000000, 54.99999999999989342, 93.75000000000004263 ) ) ;
#917 = EDGE_CURVE ( 'NONE', #6329, #7967, #176, .T. ) ;
#918 = AXIS2_PLACEMENT_3D ( 'NONE', #7982, #6026, #118 ) ;
#919 = DIRECTION ( 'NONE',  ( -0.000000000000000000, -0.000000000000000000, 1.000000000000000000 ) ) ;
#920 = ADVANCED_FACE ( 'NONE', ( #4178 ), #7961, .T. ) ;
#921 = EDGE_CURVE ( 'NONE', #3696, #7524, #4657, .T. ) ;
#922 = EDGE_CURVE ( 'NONE', #6580, #3406, #3545, .T. ) ;
#923 = VECTOR ( 'NONE', #513, 1000.000000000000000 ) ;
#924 = ORIENTED_EDGE ( 'NONE', *, *, #2528, .T. ) ;
#925 = ORIENTED_EDGE ( 'NONE', *, *, #2471, .F. ) ;
#926 = CARTESIAN_POINT ( 'NONE',  ( -125.0000000000000000, -120.0000000000000000, 0.000000000000000000 ) ) ;
#927 = AXIS2_PLACEMENT_3D ( 'NONE', #5655, #7690, #1908 ) ;
#928 = CIRCLE ( 'NONE', #1205, 5.999999999999991118 ) ;
#929 = VERTEX_POINT ( 'NONE', #6649 ) ;
#930 = CARTESIAN_POINT ( 'NONE',  ( -94.99999999999997158, -95.00000000000008527, 70.00000000000000000 ) ) ;
#931 = MANIFOLD_SOLID_BREP ( 'Boss-Extrude1', #729 ) ;
#932 = VECTOR ( 'NONE', #5994, 1000.000000000000114 ) ;
#933 = CARTESIAN_POINT ( 'NONE',  ( 55.00000000000000711, 55.00000000000001421, -56.59999999999999432 ) ) ;
#934 = CARTESIAN_POINT ( 'NONE',  ( -15.00000000000000000, 1.836970198721029589E-15, -128.0000000000000284 ) ) ;
#935 = ORIENTED_EDGE ( 'NONE', *, *, #5323, .F. ) ;
#936 = CARTESIAN_POINT ( 'NONE',  ( 9.415432556623352767, 49.10895683582204896, -4.238112224658974192 ) ) ;
#937 = EDGE_CURVE ( 'NONE', #1427, #6149, #2148, .T. ) ;
#938 = CIRCLE ( 'NONE', #2552, 75.00000000000001421 ) ;
#939 = CIRCLE ( 'NONE', #3766, 6.999999999999999112 ) ;
#940 = PLANE ( 'NONE',  #4467 ) ;
#941 = DIRECTION ( 'NONE',  ( -0.000000000000000000, -7.945337353457666666E-18, -1.000000000000000000 ) ) ;
#942 = DIRECTION ( 'NONE',  ( 0.000000000000000000, 0.000000000000000000, -1.000000000000000000 ) ) ;
#943 = DIRECTION ( 'NONE',  ( 0.000000000000000000, -0.8660254037844394848, -0.4999999999999985567 ) ) ;
#944 = VECTOR ( 'NONE', #2401, 1000.000000000000000 ) ;
#945 = AXIS2_PLACEMENT_3D ( 'NONE', #2136, #943, #2263 ) ;
#946 = EDGE_LOOP ( 'NONE', ( #1027, #5506, #399, #5076 ) ) ;
#947 = SURFACE_SIDE_STYLE ('',( #5495 ) ) ;
#948 = FACE_OUTER_BOUND ( 'NONE', #4156, .T. ) ;
#949 = EDGE_CURVE ( 'NONE', #6896, #7049, #745, .T. ) ;
#950 = MANIFOLD_SOLID_BREP ( 'Hex', #5717 ) ;
#951 = AXIS2_PLACEMENT_3D ( 'NONE', #3629, #2188, #7493 ) ;
#952 = VERTEX_POINT ( 'NONE', #3626 ) ;
#953 = AXIS2_PLACEMENT_3D ( 'NONE', #32, #3926, #724 ) ;
#954 = DIRECTION ( 'NONE',  ( 1.000000000000000000, 0.000000000000000000, 0.000000000000000000 ) ) ;
#955 = DIRECTION ( 'NONE',  ( 0.000000000000000000, 1.000000000000000000, 0.000000000000000000 ) ) ;
#956 = EDGE_LOOP ( 'NONE', ( #1669, #2525 ) ) ;
#957 = DIRECTION ( 'NONE',  ( 0.000000000000000000, 0.000000000000000000, 1.000000000000000000 ) ) ;
#958 =( NAMED_UNIT ( * ) PLANE_ANGLE_UNIT ( ) SI_UNIT ( $, .RADIAN. ) );
#959 = CARTESIAN_POINT ( 'NONE',  ( 125.0000000000000000, -120.0000000000000000, 0.000000000000000000 ) ) ;
#960 = ORIENTED_EDGE ( 'NONE', *, *, #2835, .F. ) ;
#961 = DIRECTION ( 'NONE',  ( 6.106226635438364917E-16, 3.154042683594196846E-17, 1.000000000000000000 ) ) ;
#962 = EDGE_LOOP ( 'NONE', ( #5950, #591, #6803, #1518 ) ) ;
#963 = ORIENTED_EDGE ( 'NONE', *, *, #1804, .T. ) ;
#964 = CARTESIAN_POINT ( 'NONE',  ( 115.0000000000000000, -114.9999999999999716, 0.000000000000000000 ) ) ;
#965 = DIRECTION ( 'NONE',  ( -1.000000000000000000, 0.000000000000000000, 0.000000000000000000 ) ) ;
#966 = DIRECTION ( 'NONE',  ( -0.000000000000000000, -0.000000000000000000, 1.000000000000000000 ) ) ;
#967 = DIRECTION ( 'NONE',  ( 1.000000000000000000, 0.000000000000000000, 0.000000000000000000 ) ) ;
#968 = AXIS2_PLACEMENT_3D ( 'NONE', #5784, #1269, #459 ) ;
#969 = PRODUCT_DEFINITION ( 'UNKNOWN', '', #7047, #8011 ) ;
#970 = ORIENTED_EDGE ( 'NONE', *, *, #4796, .F. ) ;
#971 = FACE_OUTER_BOUND ( 'NONE', #1682, .T. ) ;
#972 = ORIENTED_EDGE ( 'NONE', *, *, #2430, .F. ) ;
#973 = EDGE_CURVE ( 'NONE', #860, #2535, #428, .T. ) ;
#974 = DIRECTION ( 'NONE',  ( -1.000000000000000000, 0.000000000000000000, 0.000000000000000000 ) ) ;
#975 = DIRECTION ( 'NONE',  ( 1.224646799147346798E-16, 3.155443620884047222E-30, -1.000000000000000000 ) ) ;
#976 = ORIENTED_EDGE ( 'NONE', *, *, #1235, .T. ) ;
#977 = DIRECTION ( 'NONE',  ( -0.000000000000000000, -0.000000000000000000, 1.000000000000000000 ) ) ;
#978 = CARTESIAN_POINT ( 'NONE',  ( 9.999999999999998224, 8.000000000000000000, 0.000000000000000000 ) ) ;
#979 = DIRECTION ( 'NONE',  ( 1.000000000000000000, 0.000000000000000000, 0.000000000000000000 ) ) ;
#980 = EDGE_CURVE ( 'NONE', #6005, #3213, #8251, .T. ) ;
#981 = DIRECTION ( 'NONE',  ( 1.000000000000000000, 0.000000000000000000, 0.000000000000000000 ) ) ;
#982 = ADVANCED_FACE ( 'NONE', ( #4567 ), #7087, .F. ) ;
#983 = AXIS2_PLACEMENT_3D ( 'NONE', #7682, #6478, #5268 ) ;
#984 = VERTEX_POINT ( 'NONE', #1023 ) ;
#985 = CARTESIAN_POINT ( 'NONE',  ( -115.0000000000000000, 115.0000000000000000, 20.00000000000000355 ) ) ;
#986 = VERTEX_POINT ( 'NONE', #3576 ) ;
#987 = AXIS2_PLACEMENT_3D ( 'NONE', #3005, #4347, #3590 ) ;
#988 = DIRECTION ( 'NONE',  ( -0.000000000000000000, -0.000000000000000000, 1.000000000000000000 ) ) ;
#989 = DIRECTION ( 'NONE',  ( -1.000000000000000000, 0.000000000000000000, -0.000000000000000000 ) ) ;
#990 = AXIS2_PLACEMENT_3D ( 'NONE', #2437, #7757, #7107 ) ;
#991 = EDGE_CURVE ( 'NONE', #1826, #2040, #4912, .T. ) ;
#992 = CARTESIAN_POINT ( 'NONE',  ( -124.0000000000000000, -114.9999999999999858, 20.00000000000000000 ) ) ;
#993 = CARTESIAN_POINT ( 'NONE',  ( -3.243174531372579494, -49.89626761698126245, -0.4210505255250470702 ) ) ;
#994 = ORIENTED_EDGE ( 'NONE', *, *, #2184, .F. ) ;
#995 = LINE ( 'NONE', #2149, #5893 ) ;
#996 = ORIENTED_EDGE ( 'NONE', *, *, #4675, .T. ) ;
#997 = DIRECTION ( 'NONE',  ( -0.000000000000000000, -7.945337353457666666E-18, -1.000000000000000000 ) ) ;
#998 = DIRECTION ( 'NONE',  ( -0.000000000000000000, -0.000000000000000000, 1.000000000000000000 ) ) ;
#999 = DIRECTION ( 'NONE',  ( -1.000000000000000000, -2.921639538487254261E-16, 0.000000000000000000 ) ) ;
#1000 = ORIENTED_EDGE ( 'NONE', *, *, #4569, .F. ) ;
#1001 = DIRECTION ( 'NONE',  ( 1.000000000000000000, 0.000000000000000000, 0.000000000000000000 ) ) ;
#1002 = DIRECTION ( 'NONE',  ( 1.000000000000000000, 0.000000000000000000, 0.000000000000000000 ) ) ;
#1003 = ORIENTED_EDGE ( 'NONE', *, *, #8301, .T. ) ;
#1004 = PLANE ( 'NONE',  #6801 ) ;
#1005 = DIRECTION ( 'NONE',  ( 1.000000000000000000, 0.000000000000000000, 0.000000000000000000 ) ) ;
#1006 = VECTOR ( 'NONE', #4028, 1000.000000000000000 ) ;
#1007 = UNCERTAINTY_MEASURE_WITH_UNIT (LENGTH_MEASURE( 1.000000000000000082E-05 ), #7671, 'distance_accuracy_value', 'NONE');
#1008 = VERTEX_POINT ( 'NONE', #7708 ) ;
#1009 = DIRECTION ( 'NONE',  ( -0.000000000000000000, -0.000000000000000000, 1.000000000000000000 ) ) ;
#1010 = VERTEX_POINT ( 'NONE', #7054 ) ;
#1011 = DIRECTION ( 'NONE',  ( 1.000000000000000000, 0.000000000000000000, 0.000000000000000000 ) ) ;
#1012 = DIRECTION ( 'NONE',  ( -3.955169525227079253E-16, 2.675714579877178637E-31, 0.9999999999999997780 ) ) ;
#1013 = EDGE_LOOP ( 'NONE', ( #559, #6984, #2873, #7573 ) ) ;
#1014 = DIRECTION ( 'NONE',  ( -9.992007221626408864E-16, -1.000000000000000000, -0.000000000000000000 ) ) ;
#1015 = EDGE_CURVE ( 'NONE', #7541, #321, #4599, .T. ) ;
#1016 = PRODUCT_DEFINITION_SHAPE ( 'NONE', 'NONE',  #2224 ) ;
#1017 = DIRECTION ( 'NONE',  ( 0.000000000000000000, -1.224646799147353207E-16, 1.000000000000000000 ) ) ;
#1018 = ORIENTED_EDGE ( 'NONE', *, *, #3827, .T. ) ;
#1019 = CARTESIAN_POINT ( 'NONE',  ( 10.00000000000000000, -54.99999999999995026, -93.75000000000001421 ) ) ;
#1020 = ORIENTED_EDGE ( 'NONE', *, *, #2382, .F. ) ;
#1021 = PRESENTATION_STYLE_ASSIGNMENT (( #6844 ) ) ;
#1022 = ORIENTED_EDGE ( 'NONE', *, *, #5036, .F. ) ;
#1023 = CARTESIAN_POINT ( 'NONE',  ( 0.000000000000000000, 95.00000000000008527, 35.00000000000000000 ) ) ;
#1024 = EDGE_CURVE ( 'NONE', #3915, #6928, #8311, .T. ) ;
#1025 = EDGE_CURVE ( 'NONE', #6358, #4954, #6815, .T. ) ;
#1026 = EDGE_CURVE ( 'NONE', #4868, #3146, #766, .T. ) ;
#1027 = ORIENTED_EDGE ( 'NONE', *, *, #7821, .F. ) ;
#1028 = AXIS2_PLACEMENT_3D ( 'NONE', #3244, #2009, #3886 ) ;
#1029 = PLANE ( 'NONE',  #4537 ) ;
#1030 = VECTOR ( 'NONE', #5810, 1000.000000000000000 ) ;
#1031 = DIRECTION ( 'NONE',  ( 1.000000000000000000, 0.000000000000000000, 0.000000000000000000 ) ) ;
#1032 = ORIENTED_EDGE ( 'NONE', *, *, #7372, .F. ) ;
#1033 = AXIS2_PLACEMENT_3D ( 'NONE', #4475, #7026, #568 ) ;
#1034 = ORIENTED_EDGE ( 'NONE', *, *, #3154, .F. ) ;
#1035 = DIRECTION ( 'NONE',  ( 0.000000000000000000, 1.000000000000000000, 0.000000000000000000 ) ) ;
#1036 = FACE_BOUND ( 'NONE', #3299, .T. ) ;
#1037 = CARTESIAN_POINT ( 'NONE',  ( -115.0000000000000000, -115.0000000000000000, 340.0000000000000000 ) ) ;
#1038 = ORIENTED_EDGE ( 'NONE', *, *, #5870, .T. ) ;
#1039 = CIRCLE ( 'NONE', #8188, 15.00000000000000000 ) ;
#1040 = CARTESIAN_POINT ( 'NONE',  ( 120.9999999999999005, 115.0000000000000000, 0.000000000000000000 ) ) ;
#1041 = ORIENTED_EDGE ( 'NONE', *, *, #7075, .T. ) ;
#1042 = DIRECTION ( 'NONE',  ( 1.000000000000000000, 0.000000000000000000, 0.000000000000000000 ) ) ;
#1043 = CARTESIAN_POINT ( 'NONE',  ( 6.123246359811209136E-15, -49.99999999999999289, -25.00000000000000000 ) ) ;
#1044 = ORIENTED_EDGE ( 'NONE', *, *, #5451, .F. ) ;
#1045 = FACE_OUTER_BOUND ( 'NONE', #5118, .T. ) ;
#1046 = EDGE_CURVE ( 'NONE', #1156, #5510, #1993, .T. ) ;
#1047 = AXIS2_PLACEMENT_3D ( 'NONE', #6210, #2387, #6762 ) ;
#1048 = AXIS2_PLACEMENT_3D ( 'NONE', #2974, #882, #3013 ) ;
#1049 = VERTEX_POINT ( 'NONE', #727 ) ;
#1050 = CARTESIAN_POINT ( 'NONE',  ( -50.00000000000000000, -55.00000000000000000, 240.0000000000000284 ) ) ;
#1051 = ORIENTED_EDGE ( 'NONE', *, *, #6903, .T. ) ;
#1052 = DIRECTION ( 'NONE',  ( 0.000000000000000000, 0.000000000000000000, -1.000000000000000000 ) ) ;
#1053 = CARTESIAN_POINT ( 'NONE',  ( -125.0000000000000000, 125.0000000000000000, 20.00000000000000000 ) ) ;
#1054 = AXIS2_PLACEMENT_3D ( 'NONE', #285, #3489, #6881 ) ;
#1055 = ORIENTED_EDGE ( 'NONE', *, *, #2141, .T. ) ;
#1056 = CIRCLE ( 'NONE', #2670, 14.99999999999998579 ) ;
#1057 = ORIENTED_EDGE ( 'NONE', *, *, #4872, .T. ) ;
#1058 = CARTESIAN_POINT ( 'NONE',  ( 10.82846484896509409, 48.81376096915064267, -6.242155733168283760 ) ) ;
#1059 = FACE_OUTER_BOUND ( 'NONE', #4213, .T. ) ;
#1060 = AXIS2_PLACEMENT_3D ( 'NONE', #3558, #6825, #1679 ) ;
#1061 = CARTESIAN_POINT ( 'NONE',  ( -105.0000000000000000, 8.487013464091010249E-14, 20.00000000000001776 ) ) ;
#1062 = ORIENTED_EDGE ( 'NONE', *, *, #4848, .T. ) ;
#1063 = CARTESIAN_POINT ( 'NONE',  ( 114.9999999999999147, -100.0000000000000000, 250.0000000000000000 ) ) ;
#1064 = ORIENTED_EDGE ( 'NONE', *, *, #1543, .F. ) ;
#1065 = CIRCLE ( 'NONE', #799, 8.999999999999994671 ) ;
#1066 = AXIS2_PLACEMENT_3D ( 'NONE', #60, #2652, #5223 ) ;
#1067 = EDGE_LOOP ( 'NONE', ( #3144, #1132, #360, #4244, #5256, #6664, #7467, #3226 ) ) ;
#1068 = CARTESIAN_POINT ( 'NONE',  ( -60.99999999999998579, -55.00000000000000711, 27.50000000000000000 ) ) ;
#1069 = ORIENTED_EDGE ( 'NONE', *, *, #2887, .T. ) ;
#1070 = DIRECTION ( 'NONE',  ( 0.000000000000000000, 1.000000000000000000, -1.460819769243626884E-16 ) ) ;
#1071 = CARTESIAN_POINT ( 'NONE',  ( 115.0000000000000142, -115.0000000000000000, 16.39483628583463570 ) ) ;
#1072 = CIRCLE ( 'NONE', #2296, 49.99999999999998579 ) ;
#1073 = AXIS2_PLACEMENT_3D ( 'NONE', #4907, #6004, #220 ) ;
#1074 = DIRECTION ( 'NONE',  ( 0.000000000000000000, 0.000000000000000000, 1.000000000000000000 ) ) ;
#1075 = ADVANCED_FACE ( 'NONE', ( #7748 ), #1882, .T. ) ;
#1076 = EDGE_LOOP ( 'NONE', ( #5400, #6032 ) ) ;
#1077 = CARTESIAN_POINT ( 'NONE',  ( -6.271675211807169248, -49.60982880777383741, -1.656483108071704846 ) ) ;
#1078 =( NAMED_UNIT ( * ) PLANE_ANGLE_UNIT ( ) SI_UNIT ( $, .RADIAN. ) );
#1079 = FILL_AREA_STYLE_COLOUR ( '', #5193 ) ;
#1080 = AXIS2_PLACEMENT_3D ( 'NONE', #8213, #3677, #6253 ) ;
#1081 = EDGE_LOOP ( 'NONE', ( #2, #4195, #4261, #5785 ) ) ;
#1082 = AXIS2_PLACEMENT_3D ( 'NONE', #3202, #6495, #7747 ) ;
#1083 = ORIENTED_EDGE ( 'NONE', *, *, #5820, .T. ) ;
#1084 = DIRECTION ( 'NONE',  ( 1.000000000000000000, 0.000000000000000000, 0.000000000000000000 ) ) ;
#1085 = LINE ( 'NONE', #1631, #4556 ) ;
#1086 = CIRCLE ( 'NONE', #5804, 5.999999999999991118 ) ;
#1087 = VERTEX_POINT ( 'NONE', #3806 ) ;
#1088 = CARTESIAN_POINT ( 'NONE',  ( 0.000000000000000000, 125.0000000000000568, 79.99999999999992895 ) ) ;
#1089 = EDGE_CURVE ( 'NONE', #6262, #268, #5748, .T. ) ;
#1090 = DIRECTION ( 'NONE',  ( -0.000000000000000000, -0.000000000000000000, 1.000000000000000000 ) ) ;
#1091 = PRODUCT ( 'Timing Pulley', 'Timing Pulley', '', ( #7475 ) ) ;
#1092 = CARTESIAN_POINT ( 'NONE',  ( 114.9999999999999147, 99.99999999999998579, 250.0000000000000000 ) ) ;
#1093 = VERTEX_POINT ( 'NONE', #4424 ) ;
#1094 = CARTESIAN_POINT ( 'NONE',  ( 0.000000000000000000, 105.0000000000000568, 19.99999999999998934 ) ) ;
#1095 = DIRECTION ( 'NONE',  ( 1.000000000000000000, 0.000000000000000000, 0.000000000000000000 ) ) ;
#1096 = ORIENTED_EDGE ( 'NONE', *, *, #5028, .T. ) ;
#1097 = CARTESIAN_POINT ( 'NONE',  ( -109.0000000000000426, -115.0000000000000000, 20.00000000000000355 ) ) ;
#1098 = EDGE_CURVE ( 'NONE', #448, #3289, #5832, .T. ) ;
#1099 = FACE_OUTER_BOUND ( 'NONE', #5566, .T. ) ;
#1100 = EDGE_LOOP ( 'NONE', ( #2705, #116, #7783, #4128 ) ) ;
#1101 = APPLICATION_PROTOCOL_DEFINITION ( 'draft international standard', 'automotive_design', 1998, #6511 ) ;
#1102 = ORIENTED_EDGE ( 'NONE', *, *, #8208, .F. ) ;
#1103 = LINE ( 'NONE', #3662, #3498 ) ;
#1104 = LINE ( 'NONE', #3664, #3805 ) ;
#1105 = ORIENTED_EDGE ( 'NONE', *, *, #2915, .T. ) ;
#1106 = DIRECTION ( 'NONE',  ( 0.000000000000000000, 0.000000000000000000, 1.000000000000000000 ) ) ;
#1107 = VECTOR ( 'NONE', #2087, 1000.000000000000000 ) ;
#1108 = ORIENTED_EDGE ( 'NONE', *, *, #1831, .F. ) ;
#1109 = VERTEX_POINT ( 'NONE', #1317 ) ;
#1110 = CARTESIAN_POINT ( 'NONE',  ( 110.0000000000000142, 115.0000000000000000, 270.0000000000000000 ) ) ;
#1111 = CARTESIAN_POINT ( 'NONE',  ( -95.00000000000008527, 1.163414459189986590E-14, 20.00000000000000355 ) ) ;
#1112 = VERTEX_POINT ( 'NONE', #1965 ) ;
#1113 = EDGE_LOOP ( 'NONE', ( #6418, #4791, #1621, #1265 ) ) ;
#1114 = ORIENTED_EDGE ( 'NONE', *, *, #740, .F. ) ;
#1115 = ORIENTED_EDGE ( 'NONE', *, *, #3920, .T. ) ;
#1116 = DIRECTION ( 'NONE',  ( -0.000000000000000000, -0.000000000000000000, -1.000000000000000000 ) ) ;
#1117 = LINE ( 'NONE', #2431, #6840 ) ;
#1118 = AXIS2_PLACEMENT_3D ( 'NONE', #5467, #6003, #2117 ) ;
#1119 = PLANE ( 'NONE',  #1080 ) ;
#1120 = ORIENTED_EDGE ( 'NONE', *, *, #6894, .T. ) ;
#1121 = CARTESIAN_POINT ( 'NONE',  ( -125.0000000000002558, -125.0000000000000000, 0.000000000000000000 ) ) ;
#1122 = DIRECTION ( 'NONE',  ( 0.000000000000000000, 0.000000000000000000, -1.000000000000000000 ) ) ;
#1123 = VECTOR ( 'NONE', #1801, 1000.000000000000000 ) ;
#1124 = ORIENTED_EDGE ( 'NONE', *, *, #6601, .F. ) ;
#1125 = AXIS2_PLACEMENT_3D ( 'NONE', #5, #4434, #1252 ) ;
#1126 = ADVANCED_FACE ( 'NONE', ( #2059 ), #36, .T. ) ;
#1127 = DIRECTION ( 'NONE',  ( 0.000000000000000000, 1.000000000000000000, 0.000000000000000000 ) ) ;
#1128 = FACE_BOUND ( 'NONE', #2832, .T. ) ;
#1129 = ORIENTED_EDGE ( 'NONE', *, *, #2836, .T. ) ;
#1130 = DIRECTION ( 'NONE',  ( -0.000000000000000000, -7.945337353457666666E-18, -1.000000000000000000 ) ) ;
#1131 = DIRECTION ( 'NONE',  ( 0.000000000000000000, 0.000000000000000000, 1.000000000000000000 ) ) ;
#1132 = ORIENTED_EDGE ( 'NONE', *, *, #5688, .T. ) ;
#1133 = LINE ( 'NONE', #1260, #1871 ) ;
#1134 = EDGE_CURVE ( 'NONE', #5699, #3094, #5750, .T. ) ;
#1135 = EDGE_CURVE ( 'NONE', #5480, #5616, #901, .T. ) ;
#1136 = EDGE_CURVE ( 'NONE', #2735, #2791, #5195, .T. ) ;
#1137 = EDGE_LOOP ( 'NONE', ( #6698, #6760, #1494 ) ) ;
#1138 = DIRECTION ( 'NONE',  ( 0.000000000000000000, -0.4999999999999985012, 0.8660254037844393737 ) ) ;
#1139 = LINE ( 'NONE', #6232, #5220 ) ;
#1140 = ORIENTED_EDGE ( 'NONE', *, *, #7652, .T. ) ;
#1141 = DIRECTION ( 'NONE',  ( 1.321694076934710648E-16, -1.000000000000000000, 0.000000000000000000 ) ) ;
#1142 = DIRECTION ( 'NONE',  ( -0.000000000000000000, -0.000000000000000000, 1.000000000000000000 ) ) ;
#1143 = VERTEX_POINT ( 'NONE', #686 ) ;
#1144 = APPLICATION_PROTOCOL_DEFINITION ( 'draft international standard', 'automotive_design', 1998, #5219 ) ;
#1145 = ORIENTED_EDGE ( 'NONE', *, *, #664, .F. ) ;
#1146 = CARTESIAN_POINT ( 'NONE',  ( 4.999999999999994671, 0.000000000000000000, 0.000000000000000000 ) ) ;
#1147 = CARTESIAN_POINT ( 'NONE',  ( 10.40000000000000036, 0.000000000000000000, 0.000000000000000000 ) ) ;
#1148 = CIRCLE ( 'NONE', #5858, 4.999999999999990230 ) ;
#1149 = DIRECTION ( 'NONE',  ( -1.000000000000000000, 0.000000000000000000, 0.000000000000000000 ) ) ;
#1150 = ORIENTED_EDGE ( 'NONE', *, *, #1915, .F. ) ;
#1151 = CARTESIAN_POINT ( 'NONE',  ( 120.0000000000000000, 120.0000000000000000, 0.000000000000000000 ) ) ;
#1152 = CARTESIAN_POINT ( 'NONE',  ( 60.99999999999998579, -55.00000000000000711, 27.50000000000000000 ) ) ;
#1153 = ORIENTED_EDGE ( 'NONE', *, *, #2768, .T. ) ;
#1154 = CARTESIAN_POINT ( 'NONE',  ( -12.41973075191816633, 48.43322590808264039, -10.86594944112156291 ) ) ;
#1155 = ORIENTED_EDGE ( 'NONE', *, *, #7137, .F. ) ;
#1156 = VERTEX_POINT ( 'NONE', #7787 ) ;
#1157 = ADVANCED_FACE ( 'NONE', ( #2546 ), #4549, .F. ) ;
#1158 = CARTESIAN_POINT ( 'NONE',  ( 115.0000000000000000, 114.9999999999999716, 0.000000000000000000 ) ) ;
#1159 = PLANE ( 'NONE',  #4129 ) ;
#1160 = CYLINDRICAL_SURFACE ( 'NONE', #1942, 75.00000000000001421 ) ;
#1161 = PRODUCT_DEFINITION_SHAPE ( 'NONE', 'NONE',  #8353 ) ;
#1162 = LINE ( 'NONE', #2390, #1897 ) ;
#1163 = SURFACE_SIDE_STYLE ('',( #6416 ) ) ;
#1164 = CARTESIAN_POINT ( 'NONE',  ( 0.000000000000000000, 0.000000000000000000, 0.000000000000000000 ) ) ;
#1165 = EDGE_LOOP ( 'NONE', ( #6743, #6397, #4823, #4757 ) ) ;
#1166 = LINE ( 'NONE', #2919, #1123 ) ;
#1167 = DIRECTION ( 'NONE',  ( -1.752490724247359037E-17, 1.000000000000000000, 3.853078496550133260E-17 ) ) ;
#1168 = DIRECTION ( 'NONE',  ( 1.000000000000000000, 0.000000000000000000, 0.000000000000000000 ) ) ;
#1169 = CARTESIAN_POINT ( 'NONE',  ( 102.5000000000000000, 0.000000000000000000, 12.50000000000000000 ) ) ;
#1170 = DIRECTION ( 'NONE',  ( 0.000000000000000000, -0.000000000000000000, -1.000000000000000000 ) ) ;
#1171 = CARTESIAN_POINT ( 'NONE',  ( 8.557270319823464533, -49.26314968593496957, -3.379276828450694214 ) ) ;
#1172 = LINE ( 'NONE', #2644, #69 ) ;
#1173 = CIRCLE ( 'NONE', #5753, 5.999999999999991118 ) ;
#1174 = DIRECTION ( 'NONE',  ( -0.000000000000000000, -0.000000000000000000, -1.000000000000000000 ) ) ;
#1175 = ORIENTED_EDGE ( 'NONE', *, *, #6340, .F. ) ;
#1176 = ORIENTED_EDGE ( 'NONE', *, *, #7255, .T. ) ;
#1177 = CIRCLE ( 'NONE', #2781, 5.999999999999984901 ) ;
#1178 = ORIENTED_EDGE ( 'NONE', *, *, #7163, .F. ) ;
#1179 = DIRECTION ( 'NONE',  ( 1.000000000000000000, 0.000000000000000000, 0.000000000000000000 ) ) ;
#1180 = PRODUCT_RELATED_PRODUCT_CATEGORY ( 'part', '', ( #5324 ) ) ;
#1181 = ORIENTED_EDGE ( 'NONE', *, *, #460, .F. ) ;
#1182 = FACE_OUTER_BOUND ( 'NONE', #1137, .T. ) ;
#1183 = DIRECTION ( 'NONE',  ( 1.000000000000000000, 0.000000000000000000, 0.000000000000000000 ) ) ;
#1184 =( REPRESENTATION_RELATIONSHIP ('NONE','NONE', #6882, #3965 ) REPRESENTATION_RELATIONSHIP_WITH_TRANSFORMATION ( #1229 )SHAPE_REPRESENTATION_RELATIONSHIP( ) );
#1185 = EDGE_CURVE ( 'NONE', #8175, #4245, #7456, .T. ) ;
#1186 = ORIENTED_EDGE ( 'NONE', *, *, #6072, .T. ) ;
#1187 = PRODUCT_CONTEXT ( 'NONE', #77, 'mechanical' ) ;
#1188 = EDGE_CURVE ( 'NONE', #4648, #3065, #3811, .T. ) ;
#1189 = EDGE_CURVE ( 'NONE', #5618, #268, #5155, .T. ) ;
#1190 = CIRCLE ( 'NONE', #5890, 37.49999999999999289 ) ;
#1191 = DIRECTION ( 'NONE',  ( 0.000000000000000000, 0.000000000000000000, 1.000000000000000000 ) ) ;
#1192 = VECTOR ( 'NONE', #2719, 1000.000000000000000 ) ;
#1193 = EDGE_LOOP ( 'NONE', ( #3836, #2902 ) ) ;
#1194 = DIRECTION ( 'NONE',  ( -0.000000000000000000, -0.000000000000000000, 1.000000000000000000 ) ) ;
#1195 = ORIENTED_EDGE ( 'NONE', *, *, #7394, .T. ) ;
#1196 = CARTESIAN_POINT ( 'NONE',  ( 114.9999999999999147, -100.0000000000000000, 250.0000000000000000 ) ) ;
#1197 = EDGE_CURVE ( 'NONE', #4172, #3595, #4328, .T. ) ;
#1198 = CARTESIAN_POINT ( 'NONE',  ( -12.10063575899649813, 48.51393303002350166, -9.260486547765557575 ) ) ;
#1199 = VERTEX_POINT ( 'NONE', #2217 ) ;
#1200 = CIRCLE ( 'NONE', #6849, 5.499999999999991118 ) ;
#1201 = EDGE_LOOP ( 'NONE', ( #3927, #8317, #362, #71, #6233 ) ) ;
#1202 = DIRECTION ( 'NONE',  ( 1.000000000000000000, 0.000000000000000000, 0.000000000000000000 ) ) ;
#1203 = FACE_OUTER_BOUND ( 'NONE', #1797, .T. ) ;
#1204 = VECTOR ( 'NONE', #7735, 1000.000000000000000 ) ;
#1205 = AXIS2_PLACEMENT_3D ( 'NONE', #2733, #7214, #192 ) ;
#1206 = DIRECTION ( 'NONE',  ( -0.000000000000000000, -0.000000000000000000, 1.000000000000000000 ) ) ;
#1207 = VERTEX_POINT ( 'NONE', #7349 ) ;
#1208 = EDGE_CURVE ( 'NONE', #5352, #293, #1483, .T. ) ;
#1209 = ADVANCED_FACE ( 'NONE', ( #4121 ), #940, .F. ) ;
#1210 = CARTESIAN_POINT ( 'NONE',  ( 0.2517668505716685878, 2.920087862072596104E-14, -269.5025357190767181 ) ) ;
#1211 = VERTEX_POINT ( 'NONE', #1443 ) ;
#1212 = CARTESIAN_POINT ( 'NONE',  ( 1.592040838891560279E-15, 52.49999999999997868, 92.99999999999994316 ) ) ;
#1213 = CIRCLE ( 'NONE', #4702, 12.99999999999999822 ) ;
#1214 = AXIS2_PLACEMENT_3D ( 'NONE', #912, #6734, #4258 ) ;
#1215 = LINE ( 'NONE', #3138, #8195 ) ;
#1216 = DIRECTION ( 'NONE',  ( -1.000000000000000000, 0.000000000000000000, 0.000000000000000000 ) ) ;
#1217 = AXIS2_PLACEMENT_3D ( 'NONE', #4251, #1031, #955 ) ;
#1218 = CARTESIAN_POINT ( 'NONE',  ( 115.0000000000000000, -115.0000000000000000, 340.0000000000000000 ) ) ;
#1219 = DIRECTION ( 'NONE',  ( 1.000000000000000000, 0.000000000000000000, 0.000000000000000000 ) ) ;
#1220 = ORIENTED_EDGE ( 'NONE', *, *, #740, .T. ) ;
#1221 = DIRECTION ( 'NONE',  ( -1.000000000000000000, 9.992007221626408864E-16, 0.000000000000000000 ) ) ;
#1222 = VECTOR ( 'NONE', #4044, 1000.000000000000000 ) ;
#1223 = ORIENTED_EDGE ( 'NONE', *, *, #8210, .T. ) ;
#1224 = DIRECTION ( 'NONE',  ( -0.000000000000000000, -0.000000000000000000, 1.000000000000000000 ) ) ;
#1225 = ORIENTED_EDGE ( 'NONE', *, *, #1208, .F. ) ;
#1226 = DIRECTION ( 'NONE',  ( -0.000000000000000000, -0.000000000000000000, 1.000000000000000000 ) ) ;
#1227 = PLANE ( 'NONE',  #7361 ) ;
#1228 = ORIENTED_EDGE ( 'NONE', *, *, #4164, .F. ) ;
#1229 = ITEM_DEFINED_TRANSFORMATION ( 'NONE', 'NONE', #2859,  #1299 ) ;
#1230 = ORIENTED_EDGE ( 'NONE', *, *, #5274, .T. ) ;
#1231 = PLANE ( 'NONE',  #1375 ) ;
#1232 = ORIENTED_EDGE ( 'NONE', *, *, #6853, .T. ) ;
#1233 = PRODUCT_DEFINITION_SHAPE ( 'NONE', 'NONE',  #8359 ) ;
#1234 = EDGE_LOOP ( 'NONE', ( #2994, #6172, #2615, #1150, #7419, #6336 ) ) ;
#1235 = EDGE_CURVE ( 'NONE', #6452, #7276, #5560, .T. ) ;
#1236 = LINE ( 'NONE', #5104, #2277 ) ;
#1237 = ADVANCED_FACE ( 'NONE', ( #115 ), #2704, .T. ) ;
#1238 = EDGE_LOOP ( 'NONE', ( #1678, #6258, #1261 ) ) ;
#1239 = ORIENTED_EDGE ( 'NONE', *, *, #6373, .T. ) ;
#1240 = CARTESIAN_POINT ( 'NONE',  ( -8.256742446866505603, 49.31458024324043521, -3.106261761854182790 ) ) ;
#1241 = ORIENTED_EDGE ( 'NONE', *, *, #4266, .F. ) ;
#1242 = CARTESIAN_POINT ( 'NONE',  ( -114.9999999999999147, -115.0000000000000000, -28.00000000000002487 ) ) ;
#1243 = EDGE_LOOP ( 'NONE', ( #8310, #7332 ) ) ;
#1244 = AXIS2_PLACEMENT_3D ( 'NONE', #7131, #1351, #3234 ) ;
#1245 = EDGE_CURVE ( 'NONE', #6477, #2906, #6366, .T. ) ;
#1246 = DIRECTION ( 'NONE',  ( 1.000000000000000000, 0.000000000000000000, 0.000000000000000000 ) ) ;
#1247 = DIRECTION ( 'NONE',  ( 0.000000000000000000, 0.000000000000000000, 1.000000000000000000 ) ) ;
#1248 = EDGE_CURVE ( 'NONE', #5610, #6841, #1936, .T. ) ;
#1249 = DIRECTION ( 'NONE',  ( 0.000000000000000000, -1.224646799147353207E-16, 1.000000000000000000 ) ) ;
#1250 = ORIENTED_EDGE ( 'NONE', *, *, #444, .F. ) ;
#1251 = DIRECTION ( 'NONE',  ( 0.000000000000000000, -1.000000000000000000, 1.586032892321652236E-16 ) ) ;
#1252 = DIRECTION ( 'NONE',  ( 1.000000000000000000, 0.000000000000000000, 0.000000000000000000 ) ) ;
#1253 = DIRECTION ( 'NONE',  ( 0.000000000000000000, 0.000000000000000000, -1.000000000000000000 ) ) ;
#1254 = AXIS2_PLACEMENT_3D ( 'NONE', #7140, #640, #1365 ) ;
#1255 = CARTESIAN_POINT ( 'NONE',  ( 80.00000000000000000, 5.109226446042757607E-16, -4.171999999999999709 ) ) ;
#1256 = DIRECTION ( 'NONE',  ( -0.000000000000000000, -7.945337353457666666E-18, -1.000000000000000000 ) ) ;
#1257 = LINE ( 'NONE', #1984, #2389 ) ;
#1258 = PLANE ( 'NONE',  #5615 ) ;
#1259 = AXIS2_PLACEMENT_3D ( 'NONE', #645, #5115, #2551 ) ;
#1260 = CARTESIAN_POINT ( 'NONE',  ( -75.00000000000001421, 0.000000000000000000, 15.00000000000000000 ) ) ;
#1261 = ORIENTED_EDGE ( 'NONE', *, *, #871, .T. ) ;
#1262 = DIRECTION ( 'NONE',  ( 0.000000000000000000, 0.000000000000000000, 1.000000000000000000 ) ) ;
#1263 = ORIENTED_EDGE ( 'NONE', *, *, #2767, .T. ) ;
#1264 = DIRECTION ( 'NONE',  ( 1.000000000000000000, 0.000000000000000000, 0.000000000000000000 ) ) ;
#1265 = ORIENTED_EDGE ( 'NONE', *, *, #1711, .T. ) ;
#1266 = CARTESIAN_POINT ( 'NONE',  ( 110.0000000000000142, 115.0000000000000000, 270.0000000000000000 ) ) ;
#1267 = FACE_OUTER_BOUND ( 'NONE', #4745, .T. ) ;
#1268 = VERTEX_POINT ( 'NONE', #1687 ) ;
#1269 = DIRECTION ( 'NONE',  ( 0.000000000000000000, 0.000000000000000000, 1.000000000000000000 ) ) ;
#1270 = CARTESIAN_POINT ( 'NONE',  ( -75.00000000000001421, 0.000000000000000000, 0.000000000000000000 ) ) ;
#1271 = ORIENTED_EDGE ( 'NONE', *, *, #1089, .F. ) ;
#1272 = CARTESIAN_POINT ( 'NONE',  ( -1.033895191682177028E-13, -12.50000000000001066, 12.50000000000000533 ) ) ;
#1273 = EDGE_CURVE ( 'NONE', #2993, #326, #2375, .T. ) ;
#1274 = CARTESIAN_POINT ( 'NONE',  ( -11.69966253144281332, 48.61218256317027198, -16.92010850872651417 ) ) ;
#1275 = CARTESIAN_POINT ( 'NONE',  ( -102.5000000000000000, 0.000000000000000000, 0.000000000000000000 ) ) ;
#1276 = VECTOR ( 'NONE', #1311, 1000.000000000000000 ) ;
#1277 = VERTEX_POINT ( 'NONE', #7565 ) ;
#1278 = DIRECTION ( 'NONE',  ( -0.000000000000000000, -0.000000000000000000, 1.000000000000000000 ) ) ;
#1279 = DIRECTION ( 'NONE',  ( -1.000000000000000000, 0.000000000000000000, 0.000000000000000000 ) ) ;
#1280 = DIRECTION ( 'NONE',  ( -0.000000000000000000, -0.000000000000000000, 1.000000000000000000 ) ) ;
#1281 = VERTEX_POINT ( 'NONE', #7607 ) ;
#1282 = DIRECTION ( 'NONE',  ( 0.000000000000000000, 0.4999999999999984457, -0.8660254037844394848 ) ) ;
#1283 = EDGE_CURVE ( 'NONE', #5670, #323, #4893, .T. ) ;
#1284 = ADVANCED_FACE ( 'NONE', ( #3075, #1059 ), #417, .T. ) ;
#1285 = EDGE_CURVE ( 'NONE', #2048, #805, #1104, .T. ) ;
#1286 = EDGE_LOOP ( 'NONE', ( #1102, #7331, #2428 ) ) ;
#1287 = ORIENTED_EDGE ( 'NONE', *, *, #6688, .F. ) ;
#1288 = CARTESIAN_POINT ( 'NONE',  ( 4.999999999999994671, 0.000000000000000000, 0.000000000000000000 ) ) ;
#1289 = DIRECTION ( 'NONE',  ( -0.000000000000000000, 1.266875999117951024E-16, 1.000000000000000000 ) ) ;
#1290 = DIRECTION ( 'NONE',  ( -0.000000000000000000, -0.000000000000000000, 1.000000000000000000 ) ) ;
#1291 = FACE_OUTER_BOUND ( 'NONE', #6963, .T. ) ;
#1292 = DIRECTION ( 'NONE',  ( -0.000000000000000000, -0.000000000000000000, 1.000000000000000000 ) ) ;
#1293 = CARTESIAN_POINT ( 'NONE',  ( -115.0000000000000000, 115.0000000000000000, 70.00000000000000000 ) ) ;
#1294 = VERTEX_POINT ( 'NONE', #5614 ) ;
#1295 = EDGE_LOOP ( 'NONE', ( #5051, #4898, #3815, #4605 ) ) ;
#1296 = CARTESIAN_POINT ( 'NONE',  ( -114.9999999999999858, -114.9999999999999858, 10.00000000000000000 ) ) ;
#1297 = ORIENTED_EDGE ( 'NONE', *, *, #4699, .T. ) ;
#1298 = FACE_OUTER_BOUND ( 'NONE', #2580, .T. ) ;
#1299 = AXIS2_PLACEMENT_3D ( 'NONE', #5884, #1507, #5927 ) ;
#1300 = ORIENTED_EDGE ( 'NONE', *, *, #2228, .F. ) ;
#1301 = DIRECTION ( 'NONE',  ( 1.000000000000000000, 0.000000000000000000, 0.000000000000000000 ) ) ;
#1302 = FACE_OUTER_BOUND ( 'NONE', #2125, .T. ) ;
#1303 = DIRECTION ( 'NONE',  ( -0.000000000000000000, -0.000000000000000000, 1.000000000000000000 ) ) ;
#1304 = ITEM_DEFINED_TRANSFORMATION ( 'NONE', 'NONE', #7873,  #1299 ) ;
#1305 = ADVANCED_FACE ( 'NONE', ( #2420 ), #6911, .F. ) ;
#1306 = CARTESIAN_POINT ( 'NONE',  ( -1.380900529026473240E-13, 12.49999999999999822, -55.00000000000001421 ) ) ;
#1307 = ORIENTED_EDGE ( 'NONE', *, *, #3236, .F. ) ;
#1308 = VECTOR ( 'NONE', #4861, 1000.000000000000000 ) ;
#1309=STYLED_ITEM('',(#8386),#3442);
#1310 = ORIENTED_EDGE ( 'NONE', *, *, #2278, .T. ) ;
#1311 = DIRECTION ( 'NONE',  ( 1.000000000000000000, -0.000000000000000000, -0.000000000000000000 ) ) ;
#1312 = CARTESIAN_POINT ( 'NONE',  ( 0.000000000000000000, 125.0000000000000568, 79.99999999999992895 ) ) ;
#1313 = ORIENTED_EDGE ( 'NONE', *, *, #1691, .T. ) ;
#1314 = SURFACE_STYLE_USAGE ( .BOTH. , #7091 ) ;
#1315 = CIRCLE ( 'NONE', #79, 5.999999999999991118 ) ;
#1316 = ORIENTED_EDGE ( 'NONE', *, *, #5149, .T. ) ;
#1317 = CARTESIAN_POINT ( 'NONE',  ( 120.0000000000000000, 115.0000000000000000, 270.0000000000000000 ) ) ;
#1318 = AXIS2_PLACEMENT_3D ( 'NONE', #2518, #49, #5807 ) ;
#1319 = DIRECTION ( 'NONE',  ( 0.000000000000000000, 1.000000000000000000, -7.945337353457666666E-18 ) ) ;
#1320 = DIRECTION ( 'NONE',  ( -0.000000000000000000, -7.945337353457666666E-18, -1.000000000000000000 ) ) ;
#1321 = FACE_OUTER_BOUND ( 'NONE', #2841, .T. ) ;
#1322 = VECTOR ( 'NONE', #6685, 1000.000000000000000 ) ;
#1323 = CARTESIAN_POINT ( 'NONE',  ( -55.00000000000000000, -55.00000000000000000, 240.0000000000000284 ) ) ;
#1324 = CARTESIAN_POINT ( 'NONE',  ( 0.000000000000000000, 125.0000000000000568, 79.99999999999992895 ) ) ;
#1325 = ORIENTED_EDGE ( 'NONE', *, *, #5972, .F. ) ;
#1326 = FACE_OUTER_BOUND ( 'NONE', #4672, .T. ) ;
#1327 = CARTESIAN_POINT ( 'NONE',  ( 2.001832158313002451E-15, -1.040834085586084099E-14, -21.99999999999999289 ) ) ;
#1328 = AXIS2_PLACEMENT_3D ( 'NONE', #6203, #8194, #6070 ) ;
#1329 = ORIENTED_EDGE ( 'NONE', *, *, #4888, .F. ) ;
#1330 = CIRCLE ( 'NONE', #1730, 37.50000000000000000 ) ;
#1331 = ORIENTED_EDGE ( 'NONE', *, *, #6752, .T. ) ;
#1332 = CARTESIAN_POINT ( 'NONE',  ( 108.9999999999999147, 115.0000000000000000, 8.205133554287239938E-16 ) ) ;
#1333 = AXIS2_PLACEMENT_3D ( 'NONE', #3199, #3801, #595 ) ;
#1334 = FACE_OUTER_BOUND ( 'NONE', #3551, .T. ) ;
#1335 = EDGE_CURVE ( 'NONE', #2735, #4851, #7311, .T. ) ;
#1336 = CARTESIAN_POINT ( 'NONE',  ( 3.061616997868370815E-16, -2.499999999999990230, -250.0000000000000000 ) ) ;
#1337 = CYLINDRICAL_SURFACE ( 'NONE', #2260, 12.99999999999999822 ) ;
#1338 = AXIS2_PLACEMENT_3D ( 'NONE', #7250, #6573, #797 ) ;
#1339 = AXIS2_PLACEMENT_3D ( 'NONE', #3949, #1467, #3302 ) ;
#1340 = LINE ( 'NONE', #3907, #3449 ) ;
#1341 = EDGE_LOOP ( 'NONE', ( #3743, #2060, #2905, #3577 ) ) ;
#1342 = ORIENTED_EDGE ( 'NONE', *, *, #2323, .F. ) ;
#1343 = EDGE_CURVE ( 'NONE', #469, #717, #245, .T. ) ;
#1344 = ORIENTED_EDGE ( 'NONE', *, *, #6965, .F. ) ;
#1345 = DIRECTION ( 'NONE',  ( 0.000000000000000000, 0.000000000000000000, -1.000000000000000000 ) ) ;
#1346 = EDGE_CURVE ( 'NONE', #4671, #5876, #4609, .T. ) ;
#1347 = AXIS2_PLACEMENT_3D ( 'NONE', #2247, #2924, #1634 ) ;
#1348 = VECTOR ( 'NONE', #2178, 1000.000000000000000 ) ;
#1349 = EDGE_LOOP ( 'NONE', ( #1695, #7646 ) ) ;
#1350 = LINE ( 'NONE', #1266, #7264 ) ;
#1351 = DIRECTION ( 'NONE',  ( -0.000000000000000000, -0.000000000000000000, 1.000000000000000000 ) ) ;
#1352 = AXIS2_PLACEMENT_3D ( 'NONE', #2473, #566, #6940 ) ;
#1353 = ORIENTED_EDGE ( 'NONE', *, *, #6378, .F. ) ;
#1354 = CIRCLE ( 'NONE', #953, 54.99999999999995026 ) ;
#1355 = ORIENTED_EDGE ( 'NONE', *, *, #1343, .T. ) ;
#1356 = CARTESIAN_POINT ( 'NONE',  ( 54.99999999999999289, -55.00000000000000000, 216.9956969048622284 ) ) ;
#1357 = EDGE_CURVE ( 'NONE', #3406, #6580, #842, .T. ) ;
#1358 = LINE ( 'NONE', #6493, #7675 ) ;
#1359 = EDGE_CURVE ( 'NONE', #6841, #7108, #5297, .T. ) ;
#1360 = ORIENTED_EDGE ( 'NONE', *, *, #1717, .F. ) ;
#1361 = CARTESIAN_POINT ( 'NONE',  ( -102.5000000000000000, 1.347111479062088996E-15, 9.500000000000008882 ) ) ;
#1362 = ADVANCED_FACE ( 'NONE', ( #1991 ), #4621, .F. ) ;
#1363 = ORIENTED_EDGE ( 'NONE', *, *, #7635, .T. ) ;
#1364 = DIRECTION ( 'NONE',  ( -1.000000000000000000, 0.000000000000000000, 0.000000000000000000 ) ) ;
#1365 = DIRECTION ( 'NONE',  ( 0.000000000000000000, 1.000000000000000000, -7.945337353457666666E-18 ) ) ;
#1366 = ORIENTED_EDGE ( 'NONE', *, *, #7946, .F. ) ;
#1367 = FACE_BOUND ( 'NONE', #3037, .T. ) ;
#1368 = CARTESIAN_POINT ( 'NONE',  ( 124.0000000000000000, 114.9999999999999716, 20.00000000000000000 ) ) ;
#1369 = CARTESIAN_POINT ( 'NONE',  ( 0.000000000000000000, 52.49999999999997868, 79.99999999999994316 ) ) ;
#1370 = PRODUCT_DEFINITION_SHAPE ( 'NONE', 'NONE',  #8352 ) ;
#1371 = DIRECTION ( 'NONE',  ( -1.000000000000000000, -2.921639538487254261E-16, 0.000000000000000000 ) ) ;
#1372 = ORIENTED_EDGE ( 'NONE', *, *, #2788, .F. ) ;
#1373 = DIRECTION ( 'NONE',  ( -1.000000000000000000, 0.000000000000000000, 0.000000000000000000 ) ) ;
#1374 = CARTESIAN_POINT ( 'NONE',  ( -54.99999999999997868, -55.00000000000000000, -56.59999999999999432 ) ) ;
#1376 = ORIENTED_EDGE ( 'NONE', *, *, #1702, .F. ) ;
#1375 = AXIS2_PLACEMENT_3D ( 'NONE', #6364, #3156, #632 ) ;
#1377 = DIRECTION ( 'NONE',  ( 0.000000000000000000, 0.000000000000000000, -1.000000000000000000 ) ) ;
#1378 = CYLINDRICAL_SURFACE ( 'NONE', #2162, 5.999999999999991118 ) ;
#1379 = CARTESIAN_POINT ( 'NONE',  ( -59.99999999999999289, 55.00000000000000000, 220.0000000000000284 ) ) ;
#1380 =( LENGTH_UNIT ( ) NAMED_UNIT ( * ) SI_UNIT ( .MILLI., .METRE. ) );
#1381 = DIRECTION ( 'NONE',  ( -0.000000000000000000, -0.000000000000000000, 1.000000000000000000 ) ) ;
#1382 = EDGE_CURVE ( 'NONE', #7568, #7256, #5423, .T. ) ;
#1383 = ORIENTED_EDGE ( 'NONE', *, *, #1921, .F. ) ;
#1384 = DIRECTION ( 'NONE',  ( 0.000000000000000000, 1.000000000000000000, 0.000000000000000000 ) ) ;
#1385 = ORIENTED_EDGE ( 'NONE', *, *, #6069, .F. ) ;
#1386 = EDGE_LOOP ( 'NONE', ( #5814, #142 ) ) ;
#1387 = PLANE ( 'NONE',  #8067 ) ;
#1388 = CARTESIAN_POINT ( 'NONE',  ( 0.000000000000000000, 0.000000000000000000, 0.000000000000000000 ) ) ;
#1389 = LINE ( 'NONE', #5624, #1594 ) ;
#1390 = ITEM_DEFINED_TRANSFORMATION ( 'NONE', 'NONE', #1660,  #1299 ) ;
#1391 = DIRECTION ( 'NONE',  ( -1.000000000000000000, -0.000000000000000000, 0.000000000000000000 ) ) ;
#1392 = EDGE_CURVE ( 'NONE', #4954, #2252, #6357, .T. ) ;
#1393 = ADVANCED_FACE ( 'NONE', ( #3181 ), #7052, .T. ) ;
#1394 = AXIS2_PLACEMENT_3D ( 'NONE', #2395, #3731, #6308 ) ;
#1395 = DIRECTION ( 'NONE',  ( -0.000000000000000000, -1.000000000000000000, -1.224646799147353207E-16 ) ) ;
#1396 = ORIENTED_EDGE ( 'NONE', *, *, #3184, .T. ) ;
#1397 = DIRECTION ( 'NONE',  ( 0.000000000000000000, 0.000000000000000000, 1.000000000000000000 ) ) ;
#1398 = ORIENTED_EDGE ( 'NONE', *, *, #1382, .T. ) ;
#1399 = DIRECTION ( 'NONE',  ( -0.000000000000000000, -0.000000000000000000, 1.000000000000000000 ) ) ;
#1400 = ADVANCED_BREP_SHAPE_REPRESENTATION ( '', ( #3727, #1299 ), #2092 ) ;
#1401 = DIRECTION ( 'NONE',  ( 0.000000000000000000, 0.000000000000000000, 1.000000000000000000 ) ) ;
#1402 = VERTEX_POINT ( 'NONE', #5132 ) ;
#1403 = DIRECTION ( 'NONE',  ( 0.000000000000000000, 0.000000000000000000, 1.000000000000000000 ) ) ;
#1404 = CIRCLE ( 'NONE', #2867, 5.999999999999991118 ) ;
#1405 = DIRECTION ( 'NONE',  ( 0.7071067811865487940, 8.659560562354918067E-17, 0.7071067811865463515 ) ) ;
#1406 = FACE_OUTER_BOUND ( 'NONE', #6060, .T. ) ;
#1407 = CARTESIAN_POINT ( 'NONE',  ( -75.00000000000000000, 55.00000000000000711, -27.50000000000000000 ) ) ;
#1408 = ORIENTED_EDGE ( 'NONE', *, *, #7184, .F. ) ;
#1409 = DIRECTION ( 'NONE',  ( -0.000000000000000000, -0.000000000000000000, 1.000000000000000000 ) ) ;
#1410 =( NAMED_UNIT ( * ) PLANE_ANGLE_UNIT ( ) SI_UNIT ( $, .RADIAN. ) );
#1411 = LINE ( 'NONE', #6638, #932 ) ;
#1412 = VECTOR ( 'NONE', #1613, 1000.000000000000000 ) ;
#1413 = EDGE_CURVE ( 'NONE', #5147, #4486, #4874, .T. ) ;
#1414 = ORIENTED_EDGE ( 'NONE', *, *, #8095, .F. ) ;
#1415 = CARTESIAN_POINT ( 'NONE',  ( 55.00000000000000000, -55.00000000000000000, 220.0000000000000284 ) ) ;
#1416 = DIRECTION ( 'NONE',  ( 1.000000000000000000, 0.000000000000000000, 0.000000000000000000 ) ) ;
#1417 = AXIS2_PLACEMENT_3D ( 'NONE', #7031, #4519, #5124 ) ;
#1418 = DIRECTION ( 'NONE',  ( -0.000000000000000000, -0.000000000000000000, 1.000000000000000000 ) ) ;
#1419 = FILL_AREA_STYLE ('',( #2075 ) ) ;
#1420 = CARTESIAN_POINT ( 'NONE',  ( -120.9999999999999005, 115.0000000000000000, -28.00000000000002487 ) ) ;
#1421 = FACE_OUTER_BOUND ( 'NONE', #1500, .T. ) ;
#1422 = ORIENTED_EDGE ( 'NONE', *, *, #7530, .F. ) ;
#1423 = DIRECTION ( 'NONE',  ( 1.000000000000000000, 0.000000000000000000, 0.000000000000000000 ) ) ;
#1424 = EDGE_LOOP ( 'NONE', ( #7076, #1426, #8158, #1967, #7290 ) ) ;
#1425 = FACE_OUTER_BOUND ( 'NONE', #5658, .T. ) ;
#1426 = ORIENTED_EDGE ( 'NONE', *, *, #7844, .T. ) ;
#1427 = VERTEX_POINT ( 'NONE', #4098 ) ;
#1428 = CYLINDRICAL_SURFACE ( 'NONE', #5906, 4.999999999999997335 ) ;
#1429 = CARTESIAN_POINT ( 'NONE',  ( -55.00000000000000000, 55.00000000000000000, 240.0000000000000284 ) ) ;
#1430 = DIRECTION ( 'NONE',  ( 0.000000000000000000, 0.000000000000000000, 1.000000000000000000 ) ) ;
#1431 = ORIENTED_EDGE ( 'NONE', *, *, #2734, .T. ) ;
#1432 = PRODUCT_RELATED_PRODUCT_CATEGORY ( 'part', '', ( #5128 ) ) ;
#1433 = VECTOR ( 'NONE', #5737, 1000.000000000000000 ) ;
#1434 = FACE_OUTER_BOUND ( 'NONE', #2226, .T. ) ;
#1435 = VECTOR ( 'NONE', #259, 1000.000000000000000 ) ;
#1436 = VERTEX_POINT ( 'NONE', #2152 ) ;
#1437 = ADVANCED_FACE ( 'NONE', ( #7243, #6733 ), #307, .T. ) ;
#1438 = SURFACE_STYLE_USAGE ( .BOTH. , #7304 ) ;
#1439 = EDGE_CURVE ( 'NONE', #3146, #2918, #7043, .T. ) ;
#1440 = SHAPE_REPRESENTATION ( 'Upright servo motor', ( #1299 ), #7463 ) ;
#1441 = PRESENTATION_LAYER_ASSIGNMENT (  '', '', ( #5880 ) ) ;
#1442 = DIRECTION ( 'NONE',  ( 6.106226635438361958E-16, 0.000000000000000000, 1.000000000000000000 ) ) ;
#1443 = CARTESIAN_POINT ( 'NONE',  ( 59.99999999999999289, -55.00000000000000000, 220.0000000000000284 ) ) ;
#1444 = ORIENTED_EDGE ( 'NONE', *, *, #3717, .F. ) ;
#1445 = DIRECTION ( 'NONE',  ( -0.000000000000000000, -0.000000000000000000, 1.000000000000000000 ) ) ;
#1446 = VECTOR ( 'NONE', #1666, 1000.000000000000000 ) ;
#1447 = DIRECTION ( 'NONE',  ( -0.000000000000000000, -0.000000000000000000, 1.000000000000000000 ) ) ;
#1448 = EDGE_CURVE ( 'NONE', #5626, #4012, #7736, .T. ) ;
#1449 = DIRECTION ( 'NONE',  ( 1.000000000000000000, 0.000000000000000000, -0.000000000000000000 ) ) ;
#1450 = EDGE_CURVE ( 'NONE', #6338, #1207, #1511, .T. ) ;
#1451 = LINE ( 'NONE', #2709, #7830 ) ;
#1452 = ORIENTED_EDGE ( 'NONE', *, *, #5795, .T. ) ;
#1453 = FACE_BOUND ( 'NONE', #6015, .T. ) ;
#1454 = AXIS2_PLACEMENT_3D ( 'NONE', #572, #1894, #6985 ) ;
#1455 = CARTESIAN_POINT ( 'NONE',  ( 95.00000000000008527, 1.387778780781445991E-14, 35.00000000000000000 ) ) ;
#1456 = ADVANCED_FACE ( 'NONE', ( #910 ), #8038, .F. ) ;
#1457 = CIRCLE ( 'NONE', #3320, 25.00000000000000000 ) ;
#1458 = CARTESIAN_POINT ( 'NONE',  ( 125.0000000000000000, 52.49999999999997158, 0.000000000000000000 ) ) ;
#1459 = DIRECTION ( 'NONE',  ( -0.000000000000000000, -0.000000000000000000, 1.000000000000000000 ) ) ;
#1460 = AXIS2_PLACEMENT_3D ( 'NONE', #7776, #8199, #6245 ) ;
#1462 = EDGE_CURVE ( 'NONE', #1581, #15, #2602, .T. ) ;
#1461 = DIRECTION ( 'NONE',  ( 1.000000000000000000, 0.000000000000000000, 0.000000000000000000 ) ) ;
#1463 = CARTESIAN_POINT ( 'NONE',  ( 9.999999999999998224, 0.000000000000000000, 0.000000000000000000 ) ) ;
#1464 = EDGE_LOOP ( 'NONE', ( #4892, #7973, #375, #6797, #1181 ) ) ;
#1465 = AXIS2_PLACEMENT_3D ( 'NONE', #1830, #7610, #3840 ) ;
#1466 = DIRECTION ( 'NONE',  ( 1.000000000000000000, 0.000000000000000000, 0.000000000000000000 ) ) ;
#1467 = DIRECTION ( 'NONE',  ( 1.000000000000000000, 0.000000000000000000, 0.000000000000000000 ) ) ;
#1468 = ORIENTED_EDGE ( 'NONE', *, *, #7255, .F. ) ;
#1469 = CARTESIAN_POINT ( 'NONE',  ( -55.00000000000000000, -55.00000000000000000, 220.0000000000000284 ) ) ;
#1470 = DIRECTION ( 'NONE',  ( -1.000000000000000000, -0.000000000000000000, -0.000000000000000000 ) ) ;
#1471 = AXIS2_PLACEMENT_3D ( 'NONE', #3560, #7559, #361 ) ;
#1472 = VECTOR ( 'NONE', #4316, 1000.000000000000000 ) ;
#1473 = CONTEXT_DEPENDENT_SHAPE_REPRESENTATION ( #3471, #8239 ) ;
#1474 = LINE ( 'NONE', #6445, #5413 ) ;
#1475 = AXIS2_PLACEMENT_3D ( 'NONE', #1369, #3932, #5873 ) ;
#1476 = EDGE_LOOP ( 'NONE', ( #4624, #1316 ) ) ;
#1477 = LINE ( 'NONE', #7862, #1605 ) ;
#1478 = EDGE_LOOP ( 'NONE', ( #2814, #4335, #7683, #8119 ) ) ;
#1479 = CARTESIAN_POINT ( 'NONE',  ( 108.9999999999999147, 115.0000000000000000, -28.00000000000002487 ) ) ;
#1480 = AXIS2_PLACEMENT_3D ( 'NONE', #386, #2871, #1541 ) ;
#1481 =( GEOMETRIC_REPRESENTATION_CONTEXT ( 3 ) GLOBAL_UNCERTAINTY_ASSIGNED_CONTEXT ( ( #5648 ) ) GLOBAL_UNIT_ASSIGNED_CONTEXT ( ( #2505, #4543, #3802 ) ) REPRESENTATION_CONTEXT ( 'NONE', 'WORKASPACE' ) );
#1482 = PLANE ( 'NONE',  #4550 ) ;
#1483 = LINE ( 'NONE', #6755, #2989 ) ;
#1484 = EDGE_CURVE ( 'NONE', #6102, #3725, #5831, .T. ) ;
#1485 = EDGE_LOOP ( 'NONE', ( #2510, #7558, #3993, #7342, #2502 ) ) ;
#1486 = EDGE_CURVE ( 'NONE', #3309, #4072, #289, .T. ) ;
#1487 = PRODUCT_DEFINITION_SHAPE ( 'NONE', 'NONE',  #1686 ) ;
#1488 = CARTESIAN_POINT ( 'NONE',  ( -114.9999999999999147, 99.99999999999998579, 0.000000000000000000 ) ) ;
#1489 = CARTESIAN_POINT ( 'NONE',  ( -125.0000000000000000, -52.50000000000000000, 190.0000000000000284 ) ) ;
#1490 = AXIS2_PLACEMENT_3D ( 'NONE', #6464, #733, #6414 ) ;
#1491 = FACE_OUTER_BOUND ( 'NONE', #747, .T. ) ;
#1492 = DIRECTION ( 'NONE',  ( 1.000000000000000000, 0.000000000000000000, 0.000000000000000000 ) ) ;
#1493 = DIRECTION ( 'NONE',  ( -0.5000000000000042188, 1.060575238724903710E-16, -0.8660254037844361541 ) ) ;
#1494 = ORIENTED_EDGE ( 'NONE', *, *, #530, .T. ) ;
#1495 = FACE_BOUND ( 'NONE', #2408, .T. ) ;
#1496 = EDGE_LOOP ( 'NONE', ( #3327, #3854, #5221 ) ) ;
#1497 = ADVANCED_FACE ( 'NONE', ( #5339 ), #2472, .F. ) ;
#1498 = ADVANCED_FACE ( 'NONE', ( #4662 ), #3983, .F. ) ;
#1499 = ADVANCED_FACE ( 'NONE', ( #6568 ), #3346, .F. ) ;
#1500 = EDGE_LOOP ( 'NONE', ( #2987, #3974, #150, #5372 ) ) ;
#1501 = ORIENTED_EDGE ( 'NONE', *, *, #6382, .F. ) ;
#1502 = FACE_OUTER_BOUND ( 'NONE', #1234, .T. ) ;
#1503 = CARTESIAN_POINT ( 'NONE',  ( -109.5000000000000000, -114.9999999999999858, 10.00000000000000000 ) ) ;
#1504 = CARTESIAN_POINT ( 'NONE',  ( 0.000000000000000000, 0.000000000000000000, -118.0000000000000284 ) ) ;
#1505 = DIRECTION ( 'NONE',  ( -1.000000000000000000, 0.000000000000000000, -0.000000000000000000 ) ) ;
#1506 = AXIS2_PLACEMENT_3D ( 'NONE', #1146, #6279, #502 ) ;
#1507 = DIRECTION ( 'NONE',  ( 0.000000000000000000, 0.000000000000000000, 1.000000000000000000 ) ) ;
#1508 =( LENGTH_UNIT ( ) NAMED_UNIT ( * ) SI_UNIT ( .MILLI., .METRE. ) );
#1509 = LINE ( 'NONE', #4179, #8200 ) ;
#1510 = ORIENTED_EDGE ( 'NONE', *, *, #2685, .F. ) ;
#1511 = LINE ( 'NONE', #7201, #4061 ) ;
#1512 = CIRCLE ( 'NONE', #6214, 4.999999999999990230 ) ;
#1513 = CARTESIAN_POINT ( 'NONE',  ( 114.9999999999999147, 115.0000000000000000, 250.0000000000000000 ) ) ;
#1514 = FACE_OUTER_BOUND ( 'NONE', #2180, .T. ) ;
#1515 = LINE ( 'NONE', #7334, #5232 ) ;
#1516 = CARTESIAN_POINT ( 'NONE',  ( 80.00000000000000000, 0.000000000000000000, 0.000000000000000000 ) ) ;
#1517 = CARTESIAN_POINT ( 'NONE',  ( 115.0000000000000284, -115.0000000000000000, 70.00000000000000000 ) ) ;
#1518 = ORIENTED_EDGE ( 'NONE', *, *, #5972, .T. ) ;
#1519 = AXIS2_PLACEMENT_3D ( 'NONE', #197, #2821, #156 ) ;
#1520 = ORIENTED_EDGE ( 'NONE', *, *, #3187, .F. ) ;
#1521 = CARTESIAN_POINT ( 'NONE',  ( 0.000000000000000000, 0.000000000000000000, -118.0000000000000284 ) ) ;
#1522 = VERTEX_POINT ( 'NONE', #6085 ) ;
#1523 = LINE ( 'NONE', #4077, #6033 ) ;
#1524 = CARTESIAN_POINT ( 'NONE',  ( -6.274835263354055392, 49.60946935866542162, -1.658027691731842168 ) ) ;
#1525 = AXIS2_PLACEMENT_3D ( 'NONE', #2442, #6859, #5595 ) ;
#1526 = CARTESIAN_POINT ( 'NONE',  ( 0.000000000000000000, 0.000000000000000000, 20.00000000000000355 ) ) ;
#1527 = DIRECTION ( 'NONE',  ( 0.000000000000000000, 1.000000000000000000, 0.000000000000000000 ) ) ;
#1528 = DIRECTION ( 'NONE',  ( 0.000000000000000000, 0.000000000000000000, -1.000000000000000000 ) ) ;
#1529 = CARTESIAN_POINT ( 'NONE',  ( 5.000000000000000000, -4.685197434473809430, 7.372574772901430151E-15 ) ) ;
#1530 = AXIS2_PLACEMENT_3D ( 'NONE', #2669, #2062, #2013 ) ;
#1531 = CYLINDRICAL_SURFACE ( 'NONE', #1465, 5.000000000000004441 ) ;
#1532 = CARTESIAN_POINT ( 'NONE',  ( 9.999999999999994671, 0.000000000000000000, 0.000000000000000000 ) ) ;
#1533 = EDGE_CURVE ( 'NONE', #1199, #153, #4022, .T. ) ;
#1534 = VERTEX_POINT ( 'NONE', #2242 ) ;
#1535 = FACE_OUTER_BOUND ( 'NONE', #3964, .T. ) ;
#1536 = AXIS2_PLACEMENT_3D ( 'NONE', #4125, #942, #3490 ) ;
#1537 = VERTEX_POINT ( 'NONE', #139 ) ;
#1538 = ORIENTED_EDGE ( 'NONE', *, *, #5058, .F. ) ;
#1539 = DIRECTION ( 'NONE',  ( 1.000000000000000000, 0.000000000000000000, 0.000000000000000000 ) ) ;
#1540 = DIRECTION ( 'NONE',  ( 0.000000000000000000, 1.000000000000000000, 0.000000000000000000 ) ) ;
#1541 = DIRECTION ( 'NONE',  ( 0.000000000000000000, 0.000000000000000000, -1.000000000000000000 ) ) ;
#1542 = EDGE_CURVE ( 'NONE', #7555, #4076, #4780, .T. ) ;
#1543 = EDGE_CURVE ( 'NONE', #3044, #6339, #848, .T. ) ;
#1544 = LINE ( 'NONE', #6081, #387 ) ;
#1545 = EDGE_CURVE ( 'NONE', #6928, #3915, #4197, .T. ) ;
#1546 = CARTESIAN_POINT ( 'NONE',  ( 108.9999999999999147, -115.0000000000000000, 8.205133554287239938E-16 ) ) ;
#1547 = LINE ( 'NONE', #2193, #3061 ) ;
#1548 = ORIENTED_EDGE ( 'NONE', *, *, #3525, .T. ) ;
#1549 = DIRECTION ( 'NONE',  ( 0.000000000000000000, 0.000000000000000000, 1.000000000000000000 ) ) ;
#1550 = AXIS2_PLACEMENT_3D ( 'NONE', #7363, #4133, #173 ) ;
#1551 = FACE_OUTER_BOUND ( 'NONE', #7596, .T. ) ;
#1552 = ORIENTED_EDGE ( 'NONE', *, *, #1450, .T. ) ;
#1553 = ORIENTED_EDGE ( 'NONE', *, *, #1693, .F. ) ;
#1554 = DIRECTION ( 'NONE',  ( -0.000000000000000000, -0.000000000000000000, 1.000000000000000000 ) ) ;
#1555 = EDGE_CURVE ( 'NONE', #8231, #1537, #434, .T. ) ;
#1556 = EDGE_CURVE ( 'NONE', #1093, #3982, #1166, .T. ) ;
#1557 = DIRECTION ( 'NONE',  ( 1.000000000000000000, 0.000000000000000000, 0.000000000000000000 ) ) ;
#1558 =( NAMED_UNIT ( * ) PLANE_ANGLE_UNIT ( ) SI_UNIT ( $, .RADIAN. ) );
#1559 = CARTESIAN_POINT ( 'NONE',  ( -1.110223024625156540E-13, -12.49999999999999645, 1.387778780781445676E-14 ) ) ;
#1560 = ORIENTED_EDGE ( 'NONE', *, *, #3024, .T. ) ;
#1561 = CARTESIAN_POINT ( 'NONE',  ( 109.0000000000000426, -115.0000000000000000, 70.00000000000000000 ) ) ;
#1562 = VERTEX_POINT ( 'NONE', #8172 ) ;
#1563 = CARTESIAN_POINT ( 'NONE',  ( 0.000000000000000000, -115.0000000000000000, 250.0000000000000000 ) ) ;
#1564 = EDGE_CURVE ( 'NONE', #2906, #6477, #2478, .T. ) ;
#1565 = CARTESIAN_POINT ( 'NONE',  ( 102.5000000000000000, 0.000000000000000000, 12.50000000000000000 ) ) ;
#1566 = VERTEX_POINT ( 'NONE', #6176 ) ;
#1567 = CARTESIAN_POINT ( 'NONE',  ( 125.0000000000000000, 125.0000000000000000, 20.00000000000000000 ) ) ;
#1568 = DIRECTION ( 'NONE',  ( -0.000000000000000000, -0.000000000000000000, 1.000000000000000000 ) ) ;
#1569 = VECTOR ( 'NONE', #8345, 1000.000000000000000 ) ;
#1570 = LINE ( 'NONE', #160, #5897 ) ;
#1571 = DIRECTION ( 'NONE',  ( 0.000000000000000000, -1.224646799147353207E-16, 1.000000000000000000 ) ) ;
#1572 = AXIS2_PLACEMENT_3D ( 'NONE', #3282, #1924, #5869 ) ;
#1573 = PLANE ( 'NONE',  #536 ) ;
#1574 = VECTOR ( 'NONE', #7913, 1000.000000000000114 ) ;
#1575 = DIRECTION ( 'NONE',  ( -0.000000000000000000, 1.266875999117951024E-16, 1.000000000000000000 ) ) ;
#1576 = ORIENTED_EDGE ( 'NONE', *, *, #470, .T. ) ;
#1577 = ORIENTED_EDGE ( 'NONE', *, *, #2769, .T. ) ;
#1578 = VECTOR ( 'NONE', #8083, 1000.000000000000000 ) ;
#1579 = CARTESIAN_POINT ( 'NONE',  ( 10.00000000000000000, 54.99999999999989342, 93.75000000000004263 ) ) ;
#1580 = CARTESIAN_POINT ( 'NONE',  ( 99.49999999999998579, 1.530808498934191521E-15, -12.50000000000000000 ) ) ;
#1581 = VERTEX_POINT ( 'NONE', #8261 ) ;
#1582 = CARTESIAN_POINT ( 'NONE',  ( -11.21042436406065868, -48.72746226073034137, -18.04468079945885250 ) ) ;
#1583 = CIRCLE ( 'NONE', #5077, 75.00000000000001421 ) ;
#1584 = FACE_OUTER_BOUND ( 'NONE', #7774, .T. ) ;
#1585 = PRODUCT_DEFINITION ( 'UNKNOWN', '', #8277, #4878 ) ;
#1586 = AXIS2_PLACEMENT_3D ( 'NONE', #2848, #5393, #6777 ) ;
#1587 = DIRECTION ( 'NONE',  ( 0.000000000000000000, 1.000000000000000000, 0.000000000000000000 ) ) ;
#1588 = ORIENTED_EDGE ( 'NONE', *, *, #3237, .T. ) ;
#1589 = DIRECTION ( 'NONE',  ( 1.000000000000000000, 0.000000000000000000, 0.000000000000000000 ) ) ;
#1590 = EDGE_CURVE ( 'NONE', #4209, #6887, #3943, .T. ) ;
#1591 = AXIS2_PLACEMENT_3D ( 'NONE', #3931, #5710, #6978 ) ;
#1592 = FACE_OUTER_BOUND ( 'NONE', #3238, .T. ) ;
#1593 = LINE ( 'NONE', #4103, #1006 ) ;
#1594 = VECTOR ( 'NONE', #7128, 1000.000000000000000 ) ;
#1595 = DIRECTION ( 'NONE',  ( 0.000000000000000000, 0.000000000000000000, -1.000000000000000000 ) ) ;
#1596 = CARTESIAN_POINT ( 'NONE',  ( -55.00000000000000000, -55.00000000000000000, 220.0000000000000284 ) ) ;
#1597 = AXIS2_PLACEMENT_3D ( 'NONE', #4723, #1445, #2133 ) ;
#1598 = DIRECTION ( 'NONE',  ( -6.106226635438364917E-16, -3.853078496550153598E-17, -1.000000000000000000 ) ) ;
#1599 = AXIS2_PLACEMENT_3D ( 'NONE', #7278, #2142, #6512 ) ;
#1600 = ADVANCED_FACE ( 'NONE', ( #3544, #6125 ), #5512, .T. ) ;
#1601 = EDGE_LOOP ( 'NONE', ( #2907, #8094, #822 ) ) ;
#1602 = ORIENTED_EDGE ( 'NONE', *, *, #1646, .T. ) ;
#1603 = LINE ( 'NONE', #5604, #3077 ) ;
#1604 = AXIS2_PLACEMENT_3D ( 'NONE', #4532, #7083, #1301 ) ;
#1605 = VECTOR ( 'NONE', #2094, 1000.000000000000000 ) ;
#1606 = ORIENTED_EDGE ( 'NONE', *, *, #3419, .F. ) ;
#1607 = CARTESIAN_POINT ( 'NONE',  ( 0.000000000000000000, 0.000000000000000000, -28.00000000000002487 ) ) ;
#1608 = DIRECTION ( 'NONE',  ( 1.000000000000000000, 0.000000000000000000, 0.000000000000000000 ) ) ;
#1609 = ORIENTED_EDGE ( 'NONE', *, *, #6476, .F. ) ;
#1610 = CARTESIAN_POINT ( 'NONE',  ( -108.9999999999999147, 115.0000000000000000, -28.00000000000002487 ) ) ;
#1611 = CONICAL_SURFACE ( 'NONE', #7408, 4.171999999999999709, 0.7853981633975609666 ) ;
#1612 = DIRECTION ( 'NONE',  ( -1.000000000000000000, 0.000000000000000000, 0.000000000000000000 ) ) ;
#1613 = DIRECTION ( 'NONE',  ( -0.000000000000000000, -1.000000000000000000, -0.000000000000000000 ) ) ;
#1614 = FACE_OUTER_BOUND ( 'NONE', #3031, .T. ) ;
#1615 = CARTESIAN_POINT ( 'NONE',  ( 120.5000000000000000, 114.9999999999999716, 20.00000000000000000 ) ) ;
#1616 = VECTOR ( 'NONE', #7534, 1000.000000000000000 ) ;
#1617 = VECTOR ( 'NONE', #3669, 1000.000000000000000 ) ;
#1618 = VERTEX_POINT ( 'NONE', #2962 ) ;
#1619 = ORIENTED_EDGE ( 'NONE', *, *, #2976, .F. ) ;
#1620 = CIRCLE ( 'NONE', #7960, 75.00000000000001421 ) ;
#1621 = ORIENTED_EDGE ( 'NONE', *, *, #7009, .T. ) ;
#1622 = AXIS2_PLACEMENT_3D ( 'NONE', #2587, #6337, #5791 ) ;
#1623 = DIRECTION ( 'NONE',  ( -1.000000000000000000, -0.000000000000000000, -0.000000000000000000 ) ) ;
#1624 = PLANE ( 'NONE',  #2738 ) ;
#1625 = DIRECTION ( 'NONE',  ( 1.000000000000000000, 0.000000000000000000, 0.000000000000000000 ) ) ;
#1626 = VERTEX_POINT ( 'NONE', #5552 ) ;
#1627 = CARTESIAN_POINT ( 'NONE',  ( -0.8294483708339484007, -50.00000000000000711, -7.623296525288703052E-18 ) ) ;
#1628 = DIRECTION ( 'NONE',  ( 0.000000000000000000, 0.000000000000000000, -1.000000000000000000 ) ) ;
#1629 = FACE_OUTER_BOUND ( 'NONE', #264, .T. ) ;
#1630 = ORIENTED_EDGE ( 'NONE', *, *, #7051, .T. ) ;
#1631 = CARTESIAN_POINT ( 'NONE',  ( 95.00000000000002842, -95.00000000000002842, 35.00000000000000000 ) ) ;
#1632 = EDGE_LOOP ( 'NONE', ( #4319, #5593, #637, #1129, #7242 ) ) ;
#1633 = ORIENTED_EDGE ( 'NONE', *, *, #3223, .T. ) ;
#1634 = DIRECTION ( 'NONE',  ( 1.000000000000000000, 0.000000000000000000, 0.000000000000000000 ) ) ;
#1635 = DIRECTION ( 'NONE',  ( -0.000000000000000000, -0.000000000000000000, -1.000000000000000000 ) ) ;
#1636 = EDGE_CURVE ( 'NONE', #3543, #5352, #2216, .T. ) ;
#1637 = ORIENTED_EDGE ( 'NONE', *, *, #444, .T. ) ;
#1638 = DIRECTION ( 'NONE',  ( -1.000000000000000000, -0.000000000000000000, -0.000000000000000000 ) ) ;
#1639 = CIRCLE ( 'NONE', #6351, 75.00000000000001421 ) ;
#1640 = ORIENTED_EDGE ( 'NONE', *, *, #1555, .F. ) ;
#1641 = ORIENTED_EDGE ( 'NONE', *, *, #4698, .F. ) ;
#1642 = CARTESIAN_POINT ( 'NONE',  ( 0.000000000000000000, 4.500000000000000000, -28.00000000000002487 ) ) ;
#1643 = EDGE_CURVE ( 'NONE', #6249, #5775, #7359, .T. ) ;
#1644 = ORIENTED_EDGE ( 'NONE', *, *, #5930, .T. ) ;
#1645 = DIRECTION ( 'NONE',  ( -0.000000000000000000, -0.000000000000000000, 1.000000000000000000 ) ) ;
#1646 = EDGE_CURVE ( 'NONE', #3602, #4182, #8060, .T. ) ;
#1647 = EDGE_CURVE ( 'NONE', #4789, #3289, #5301, .T. ) ;
#1648 = ORIENTED_EDGE ( 'NONE', *, *, #5870, .F. ) ;
#1649 = DIRECTION ( 'NONE',  ( 0.8571673007021134438, 0.000000000000000000, 0.5150380749100522682 ) ) ;
#1650 = DIRECTION ( 'NONE',  ( 6.106226635438361958E-16, 0.000000000000000000, 1.000000000000000000 ) ) ;
#1651 = DIRECTION ( 'NONE',  ( -1.000000000000000000, -0.000000000000000000, -0.000000000000000000 ) ) ;
#1652 = CARTESIAN_POINT ( 'NONE',  ( -120.4999999999999858, -114.9999999999999858, 10.00000000000000000 ) ) ;
#1653 = CARTESIAN_POINT ( 'NONE',  ( 0.000000000000000000, -125.0000000000000000, -12.50000000000000000 ) ) ;
#1654 = ORIENTED_EDGE ( 'NONE', *, *, #2229, .F. ) ;
#1655 = EDGE_CURVE ( 'NONE', #6306, #986, #7595, .T. ) ;
#1656 = VERTEX_POINT ( 'NONE', #5197 ) ;
#1657 = ORIENTED_EDGE ( 'NONE', *, *, #1392, .T. ) ;
#1658 = FACE_OUTER_BOUND ( 'NONE', #1067, .T. ) ;
#1659 = CARTESIAN_POINT ( 'NONE',  ( -99.99999999999990052, 115.0000000000000000, 250.0000000000000000 ) ) ;
#1660 = AXIS2_PLACEMENT_3D ( 'NONE', #6785, #4561, #4844 ) ;
#1661 = LINE ( 'NONE', #339, #5798 ) ;
#1662 = VERTEX_POINT ( 'NONE', #5987 ) ;
#1663 = ADVANCED_FACE ( 'NONE', ( #3888, #2011, #6544, #5286, #3359 ), #158, .F. ) ;
#1664 = DIRECTION ( 'NONE',  ( -1.000000000000000000, -2.921639538487254261E-16, 0.000000000000000000 ) ) ;
#1665 = VERTEX_POINT ( 'NONE', #7350 ) ;
#1666 = DIRECTION ( 'NONE',  ( -0.000000000000000000, -0.000000000000000000, -1.000000000000000000 ) ) ;
#1667 = CLOSED_SHELL ( 'NONE', ( #2679, #1880, #7336, #2122, #6642, #3883, #8031, #3707, #824, #6804, #606, #5668, #52, #4927, #1815, #5762, #393, #2091, #529, #4372, #8145, #2776, #6343, #204, #3859, #1600, #7114, #6811, #2441, #3318, #560, #4099, #1456, #1497, #6513 ) ) ;
#1668 = CARTESIAN_POINT ( 'NONE',  ( -94.99999999999997158, -95.00000000000008527, 70.00000000000000000 ) ) ;
#1669 = ORIENTED_EDGE ( 'NONE', *, *, #6182, .F. ) ;
#1670 = DIRECTION ( 'NONE',  ( 0.000000000000000000, 0.000000000000000000, -1.000000000000000000 ) ) ;
#1671 = EDGE_LOOP ( 'NONE', ( #3004, #2889, #8068, #4799 ) ) ;
#1672 = CYLINDRICAL_SURFACE ( 'NONE', #4564, 12.99999999999999822 ) ;
#1673 = DIRECTION ( 'NONE',  ( 1.000000000000000000, 0.000000000000000000, 0.000000000000000000 ) ) ;
#1674 = CARTESIAN_POINT ( 'NONE',  ( 120.5000000000000000, -114.9999999999999716, 0.000000000000000000 ) ) ;
#1675 = CARTESIAN_POINT ( 'NONE',  ( -75.00000000000000000, -54.99999999999999289, 27.50000000000000000 ) ) ;
#1676 = DIRECTION ( 'NONE',  ( 1.000000000000000000, 0.000000000000000000, 0.000000000000000000 ) ) ;
#1677 = CIRCLE ( 'NONE', #8291, 5.999999999999991118 ) ;
#1678 = ORIENTED_EDGE ( 'NONE', *, *, #6853, .F. ) ;
#1679 = DIRECTION ( 'NONE',  ( 0.000000000000000000, 0.000000000000000000, -1.000000000000000000 ) ) ;
#1680 = VERTEX_POINT ( 'NONE', #4849 ) ;
#1681 = PLANE ( 'NONE',  #3756 ) ;
#1682 = EDGE_LOOP ( 'NONE', ( #8203, #4102, #5975, #2895 ) ) ;
#1683 = SHAPE_DEFINITION_REPRESENTATION ( #1016, #4267 ) ;
#1684 = ORIENTED_EDGE ( 'NONE', *, *, #2388, .T. ) ;
#1685 = DIRECTION ( 'NONE',  ( -0.000000000000000000, -1.000000000000000000, -0.000000000000000000 ) ) ;
#1686 = PRODUCT_DEFINITION ( 'UNKNOWN', '', #2343, #7430 ) ;
#1687 = CARTESIAN_POINT ( 'NONE',  ( 9.999999999999994671, 9.797174393178825657E-16, -8.000000000000000000 ) ) ;
#1688 = VECTOR ( 'NONE', #6126, 1000.000000000000000 ) ;
#1689 = ORIENTED_EDGE ( 'NONE', *, *, #6534, .T. ) ;
#1690 = CARTESIAN_POINT ( 'NONE',  ( -115.0000000000000000, -115.0000000000000000, 270.0000000000000000 ) ) ;
#1691 = EDGE_CURVE ( 'NONE', #5627, #402, #6915, .T. ) ;
#1692 = DIRECTION ( 'NONE',  ( -1.752490724247359037E-17, 1.000000000000000000, 3.853078496550133260E-17 ) ) ;
#1693 = EDGE_CURVE ( 'NONE', #5775, #2457, #5565, .T. ) ;
#1694 = DIRECTION ( 'NONE',  ( 1.000000000000000000, 0.000000000000000000, 0.000000000000000000 ) ) ;
#1695 = ORIENTED_EDGE ( 'NONE', *, *, #189, .T. ) ;
#1696 = ORIENTED_EDGE ( 'NONE', *, *, #715, .T. ) ;
#1697 = ORIENTED_EDGE ( 'NONE', *, *, #3134, .T. ) ;
#1698 = EDGE_CURVE ( 'NONE', #3530, #2214, #6790, .T. ) ;
#1699 = DIRECTION ( 'NONE',  ( 1.000000000000000000, 0.000000000000000000, 0.000000000000000000 ) ) ;
#1700 = ADVANCED_FACE ( 'NONE', ( #6744 ), #8096, .F. ) ;
#1701 = DIRECTION ( 'NONE',  ( -0.000000000000000000, -0.000000000000000000, -1.000000000000000000 ) ) ;
#1702 = EDGE_CURVE ( 'NONE', #1581, #6149, #490, .T. ) ;
#1703 = CIRCLE ( 'NONE', #4107, 9.000000000000007105 ) ;
#1704 = AXIS2_PLACEMENT_3D ( 'NONE', #2605, #5723, #8304 ) ;
#1705 = DIRECTION ( 'NONE',  ( -1.752490724247359037E-17, 1.000000000000000000, 3.853078496550133260E-17 ) ) ;
#1706 = VERTEX_POINT ( 'NONE', #4397 ) ;
#1707 = CARTESIAN_POINT ( 'NONE',  ( -12.09737906851130518, -48.51474822866212122, -15.75174765218248574 ) ) ;
#1708 = SHAPE_REPRESENTATION ( 'Lid', ( #1299 ), #3387 ) ;
#1709 = AXIS2_PLACEMENT_3D ( 'NONE', #4046, #7188, #5252 ) ;
#1710 = ORIENTED_EDGE ( 'NONE', *, *, #6741, .T. ) ;
#1711 = EDGE_CURVE ( 'NONE', #929, #501, #3521, .T. ) ;
#1712 = PLANE ( 'NONE',  #6288 ) ;
#1713 = CARTESIAN_POINT ( 'NONE',  ( 80.00000000000000000, 0.000000000000000000, 0.000000000000000000 ) ) ;
#1714 = ORIENTED_EDGE ( 'NONE', *, *, #3909, .F. ) ;
#1715 = CIRCLE ( 'NONE', #7657, 5.999999999999991118 ) ;
#1716 = CARTESIAN_POINT ( 'NONE',  ( -115.0000000000000000, 115.0000000000000000, 270.0000000000000000 ) ) ;
#1717 = EDGE_CURVE ( 'NONE', #6640, #1836, #155, .T. ) ;
#1718 = CARTESIAN_POINT ( 'NONE',  ( -95.00000000000001421, 0.000000000000000000, 15.00000000000000000 ) ) ;
#1719 = DIRECTION ( 'NONE',  ( -0.000000000000000000, -0.000000000000000000, -1.000000000000000000 ) ) ;
#1720 = AXIS2_PLACEMENT_3D ( 'NONE', #4653, #6681, #4610 ) ;
#1721 = AXIS2_PLACEMENT_3D ( 'NONE', #7158, #95, #6475 ) ;
#1722 = ORIENTED_EDGE ( 'NONE', *, *, #7897, .T. ) ;
#1723 = LINE ( 'NONE', #4756, #3086 ) ;
#1724 = ORIENTED_EDGE ( 'NONE', *, *, #5346, .T. ) ;
#1725 = DIRECTION ( 'NONE',  ( 0.000000000000000000, 0.000000000000000000, 1.000000000000000000 ) ) ;
#1726 = CARTESIAN_POINT ( 'NONE',  ( 125.0000000000000000, 125.0000000000000568, -9.184850993605156622E-15 ) ) ;
#1727 = AXIS2_PLACEMENT_3D ( 'NONE', #4123, #7941, #7907 ) ;
#1728 = EDGE_LOOP ( 'NONE', ( #232, #5693, #3645, #5839 ) ) ;
#1729 = APPLICATION_PROTOCOL_DEFINITION ( 'draft international standard', 'automotive_design', 1998, #6561 ) ;
#1730 = AXIS2_PLACEMENT_3D ( 'NONE', #423, #3269, #2425 ) ;
#1731 = EDGE_LOOP ( 'NONE', ( #7387, #5133, #8189, #1619 ) ) ;
#1732 = DIRECTION ( 'NONE',  ( -1.000000000000000000, -0.000000000000000000, -0.000000000000000000 ) ) ;
#1733 = VECTOR ( 'NONE', #5059, 1000.000000000000000 ) ;
#1734 = ORIENTED_EDGE ( 'NONE', *, *, #5795, .F. ) ;
#1735 = DIRECTION ( 'NONE',  ( -0.000000000000000000, -0.000000000000000000, -1.000000000000000000 ) ) ;
#1736 = VECTOR ( 'NONE', #7864, 1000.000000000000000 ) ;
#1737 = ORIENTED_EDGE ( 'NONE', *, *, #443, .F. ) ;
#1738 = EDGE_LOOP ( 'NONE', ( #3789, #2490, #5915, #3472 ) ) ;
#1739 = DIRECTION ( 'NONE',  ( -0.000000000000000000, -0.000000000000000000, 1.000000000000000000 ) ) ;
#1740 = CARTESIAN_POINT ( 'NONE',  ( -114.9999999999999716, 114.9999999999999858, 10.00000000000000000 ) ) ;
#1741 = ORIENTED_EDGE ( 'NONE', *, *, #2196, .F. ) ;
#1742 = AXIS2_PLACEMENT_3D ( 'NONE', #2367, #4918, #4885 ) ;
#1743 = VECTOR ( 'NONE', #4143, 1000.000000000000000 ) ;
#1744 = EDGE_CURVE ( 'NONE', #3799, #4692, #4066, .T. ) ;
#1745 = EDGE_CURVE ( 'NONE', #7187, #2575, #4891, .T. ) ;
#1746 = EDGE_LOOP ( 'NONE', ( #2201, #2378 ) ) ;
#1747 = EDGE_LOOP ( 'NONE', ( #5047, #7771, #6216, #6700 ) ) ;
#1748 = DIRECTION ( 'NONE',  ( 0.000000000000000000, 0.000000000000000000, 1.000000000000000000 ) ) ;
#1749 = DIRECTION ( 'NONE',  ( 1.000000000000000000, 0.000000000000000000, 0.000000000000000000 ) ) ;
#1750 = VECTOR ( 'NONE', #7803, 1000.000000000000000 ) ;
#1751 = AXIS2_PLACEMENT_3D ( 'NONE', #1805, #2063, #7837 ) ;
#1752 = ADVANCED_FACE ( 'NONE', ( #7099 ), #3846, .F. ) ;
#1753 = LINE ( 'NONE', #2434, #2301 ) ;
#1754 = EDGE_LOOP ( 'NONE', ( #5016, #1300, #6482, #2342 ) ) ;
#1755 = DIRECTION ( 'NONE',  ( -1.000000000000000000, 0.000000000000000000, 0.000000000000000000 ) ) ;
#1756 = ADVANCED_FACE ( 'NONE', ( #1321 ), #1160, .F. ) ;
#1757 = ADVANCED_FACE ( 'NONE', ( #3722 ), #3166, .F. ) ;
#1758 = SURFACE_STYLE_FILL_AREA ( #3003 ) ;
#1759 = EDGE_CURVE ( 'NONE', #3837, #1946, #3323, .T. ) ;
#1760 = AXIS2_PLACEMENT_3D ( 'NONE', #4212, #4859, #4093 ) ;
#1761 = VECTOR ( 'NONE', #6971, 1000.000000000000000 ) ;
#1762 = ORIENTED_EDGE ( 'NONE', *, *, #2056, .T. ) ;
#1763 = CARTESIAN_POINT ( 'NONE',  ( -115.0000000000000000, 115.0000000000000000, 70.00000000000000000 ) ) ;
#1764 = FACE_BOUND ( 'NONE', #612, .T. ) ;
#1765 = LINE ( 'NONE', #6220, #6456 ) ;
#1766 = VECTOR ( 'NONE', #3795, 1000.000000000000000 ) ;
#1767 = DIRECTION ( 'NONE',  ( -1.000000000000000000, 0.000000000000000000, 0.000000000000000000 ) ) ;
#1768 = ORIENTED_EDGE ( 'NONE', *, *, #4192, .T. ) ;
#1769 = FACE_OUTER_BOUND ( 'NONE', #7750, .T. ) ;
#1770 = CARTESIAN_POINT ( 'NONE',  ( 6.260380647299085055, -49.60786550102538683, -23.32709356835264103 ) ) ;
#1771 = PRODUCT_DEFINITION_SHAPE ( 'NONE', 'NONE',  #8361 ) ;
#1772 = CARTESIAN_POINT ( 'NONE',  ( 0.000000000000000000, 0.000000000000000000, -248.3416876048222832 ) ) ;
#1773 = ORIENTED_EDGE ( 'NONE', *, *, #396, .T. ) ;
#1774 = CARTESIAN_POINT ( 'NONE',  ( 102.5000000000000000, 0.000000000000000000, 12.50000000000000000 ) ) ;
#1775 = CARTESIAN_POINT ( 'NONE',  ( 0.000000000000000000, -125.0000000000000568, 79.99999999999997158 ) ) ;
#1776 = ORIENTED_EDGE ( 'NONE', *, *, #4676, .F. ) ;
#1777 = FACE_OUTER_BOUND ( 'NONE', #3624, .T. ) ;
#1778 = CARTESIAN_POINT ( 'NONE',  ( 5.000000000000000000, 7.027796151710712813, -4.057500000000006324 ) ) ;
#1779 = SHAPE_DEFINITION_REPRESENTATION ( #1487, #1708 ) ;
#1780 = EDGE_CURVE ( 'NONE', #5976, #2287, #7789, .T. ) ;
#1781 = CARTESIAN_POINT ( 'NONE',  ( 9.126495132297687718, 49.16089547422080130, -21.05129937300930010 ) ) ;
#1782 = ORIENTED_EDGE ( 'NONE', *, *, #6074, .T. ) ;
#1783 = EDGE_LOOP ( 'NONE', ( #8289, #4269, #7405, #2363 ) ) ;
#1784 = CARTESIAN_POINT ( 'NONE',  ( 14.14213562373095279, -5.000000000000000000, 0.000000000000000000 ) ) ;
#1785 = CYLINDRICAL_SURFACE ( 'NONE', #1873, 75.00000000000001421 ) ;
#1786 = AXIS2_PLACEMENT_3D ( 'NONE', #8007, #8046, #272 ) ;
#1787 = VERTEX_POINT ( 'NONE', #3399 ) ;
#1788 = ORIENTED_EDGE ( 'NONE', *, *, #1439, .T. ) ;
#1789 = PLANE ( 'NONE',  #4547 ) ;
#1790 = PLANE ( 'NONE',  #3594 ) ;
#1791 = ORIENTED_EDGE ( 'NONE', *, *, #1450, .F. ) ;
#1792 = ORIENTED_EDGE ( 'NONE', *, *, #3763, .F. ) ;
#1793 = CARTESIAN_POINT ( 'NONE',  ( 125.0000000000000000, -125.0000000000000284, 70.00000000000000000 ) ) ;
#1794 = LINE ( 'NONE', #3627, #6152 ) ;
#1795 = AXIS2_PLACEMENT_3D ( 'NONE', #3418, #3382, #872 ) ;
#1796 = CARTESIAN_POINT ( 'NONE',  ( 105.0000000000000000, -105.0000000000000568, 240.0000000000000284 ) ) ;
#1797 = EDGE_LOOP ( 'NONE', ( #6153, #2426, #2650, #2275 ) ) ;
#1798 = CARTESIAN_POINT ( 'NONE',  ( -0.4088724290315628451, -49.99999999999999289, -25.00000000000000000 ) ) ;
#1799 = DIRECTION ( 'NONE',  ( 1.110223024625156540E-16, -1.000000000000000000, 1.033438071402920287E-30 ) ) ;
#1800 = VECTOR ( 'NONE', #4904, 1000.000000000000000 ) ;
#1801 = DIRECTION ( 'NONE',  ( 1.000000000000000000, 0.000000000000000000, 0.000000000000000000 ) ) ;
#1802 = CARTESIAN_POINT ( 'NONE',  ( 95.00000000000000000, 95.00000000000008527, 70.00000000000000000 ) ) ;
#1803 = EDGE_CURVE ( 'NONE', #2287, #6267, #4623, .T. ) ;
#1804 = EDGE_CURVE ( 'NONE', #378, #7416, #731, .T. ) ;
#1805 = CARTESIAN_POINT ( 'NONE',  ( 54.99999999999999289, 55.00000000000000711, -27.50000000000000000 ) ) ;
#1806 = EDGE_CURVE ( 'NONE', #4162, #3924, #4896, .T. ) ;
#1807 = LINE ( 'NONE', #1040, #8016 ) ;
#1808 = CARTESIAN_POINT ( 'NONE',  ( 0.000000000000000000, 115.0000000000000000, 250.0000000000000000 ) ) ;
#1809 = VECTOR ( 'NONE', #3841, 1000.000000000000000 ) ;
#1810 = ORIENTED_EDGE ( 'NONE', *, *, #5085, .T. ) ;
#1811 = SURFACE_SIDE_STYLE ('',( #2404 ) ) ;
#1812 = ADVANCED_BREP_SHAPE_REPRESENTATION ( '', ( #6502, #1299 ), #205 ) ;
#1813 = SPHERICAL_SURFACE ( 'NONE', #3588, 3.000000000000001776 ) ;
#1814 = AXIS2_PLACEMENT_3D ( 'NONE', #3162, #8332, #5070 ) ;
#1815 = ADVANCED_FACE ( 'NONE', ( #7307 ), #4081, .T. ) ;
#1816 = ORIENTED_EDGE ( 'NONE', *, *, #1283, .T. ) ;
#1817 = EDGE_CURVE ( 'NONE', #6862, #1662, #6546, .T. ) ;
#1818 = CARTESIAN_POINT ( 'NONE',  ( -120.9999999999999005, -115.0000000000000000, -28.00000000000002487 ) ) ;
#1819 = CARTESIAN_POINT ( 'NONE',  ( 120.0000000000000000, -115.0000000000000000, 340.0000000000000000 ) ) ;
#1820 = EDGE_LOOP ( 'NONE', ( #4840, #1734, #409 ) ) ;
#1821 = LINE ( 'NONE', #4366, #7542 ) ;
#1822 = DIRECTION ( 'NONE',  ( -0.000000000000000000, -0.000000000000000000, 1.000000000000000000 ) ) ;
#1823 = CIRCLE ( 'NONE', #3960, 4.999999999999990230 ) ;
#1824 = ITEM_DEFINED_TRANSFORMATION ( 'NONE', 'NONE', #165,  #1299 ) ;
#1825 = CARTESIAN_POINT ( 'NONE',  ( 20.76917701662883076, -5.000000000000000000, 57.99999999999999289 ) ) ;
#1826 = VERTEX_POINT ( 'NONE', #2707 ) ;
#1827 = CARTESIAN_POINT ( 'NONE',  ( -7.743805596760466869E-14, -12.49999999999999467, 54.99999999999997868 ) ) ;
#1828 = MECHANICAL_DESIGN_GEOMETRIC_PRESENTATION_REPRESENTATION (  '', ( #3014 ), #4768 ) ;
#1829 = ADVANCED_FACE ( 'NONE', ( #5289, #5255 ), #3937, .F. ) ;
#1830 = CARTESIAN_POINT ( 'NONE',  ( -120.0000000000000000, 120.0000000000000000, -28.00000000000002487 ) ) ;
#1831 = EDGE_CURVE ( 'NONE', #900, #7564, #7396, .T. ) ;
#1832 = ORIENTED_EDGE ( 'NONE', *, *, #6250, .F. ) ;
#1833 = LINE ( 'NONE', #6369, #391 ) ;
#1834 = AXIS2_PLACEMENT_3D ( 'NONE', #3414, #5999, #216 ) ;
#1835 = CARTESIAN_POINT ( 'NONE',  ( -9.920070434648176061, 49.00675803034337008, -20.11641848348689976 ) ) ;
#1836 = VERTEX_POINT ( 'NONE', #4048 ) ;
#1837 = ORIENTED_EDGE ( 'NONE', *, *, #3482, .T. ) ;
#1838 = DIRECTION ( 'NONE',  ( 0.000000000000000000, 0.000000000000000000, -1.000000000000000000 ) ) ;
#1839 = FACE_OUTER_BOUND ( 'NONE', #7122, .T. ) ;
#1840 = DIRECTION ( 'NONE',  ( -0.000000000000000000, -1.000000000000000000, 1.586032892321652236E-16 ) ) ;
#1841 = DIRECTION ( 'NONE',  ( 0.000000000000000000, -1.000000000000000000, 9.256405414277014607E-16 ) ) ;
#1842 = ORIENTED_EDGE ( 'NONE', *, *, #1698, .T. ) ;
#1843 = CYLINDRICAL_SURFACE ( 'NONE', #2399, 5.999999999999991118 ) ;
#1844 = DIRECTION ( 'NONE',  ( 0.000000000000000000, 1.000000000000000000, 0.000000000000000000 ) ) ;
#1845 = LINE ( 'NONE', #8344, #3612 ) ;
#1846 = CARTESIAN_POINT ( 'NONE',  ( 12.10063575899649990, -48.51393303002349455, -9.260486547765564680 ) ) ;
#1847 = DIRECTION ( 'NONE',  ( -0.000000000000000000, -1.000000000000000000, 1.586032892321652236E-16 ) ) ;
#1848 = AXIS2_PLACEMENT_3D ( 'NONE', #45, #7313, #3973 ) ;
#1849 = CIRCLE ( 'NONE', #6559, 75.00000000000001421 ) ;
#1850 = LINE ( 'NONE', #2451, #2663 ) ;
#1851 = EDGE_CURVE ( 'NONE', #1836, #2601, #1411, .T. ) ;
#1852 = ORIENTED_EDGE ( 'NONE', *, *, #7492, .T. ) ;
#1853 = DIRECTION ( 'NONE',  ( 0.000000000000000000, 0.000000000000000000, 1.000000000000000000 ) ) ;
#1854 = AXIS2_PLACEMENT_3D ( 'NONE', #4858, #5664, #6078 ) ;
#1855 = UNCERTAINTY_MEASURE_WITH_UNIT (LENGTH_MEASURE( 1.000000000000000082E-05 ), #3540, 'distance_accuracy_value', 'NONE');
#1856 = ORIENTED_EDGE ( 'NONE', *, *, #6275, .T. ) ;
#1857 = DIRECTION ( 'NONE',  ( -0.8571673007021116675, 1.049727191138617833E-16, 0.5150380749100552658 ) ) ;
#1858 = FACE_BOUND ( 'NONE', #485, .T. ) ;
#1859 = EDGE_LOOP ( 'NONE', ( #789, #2881, #5851, #4229, #5350 ) ) ;
#1860 = CARTESIAN_POINT ( 'NONE',  ( 0.000000000000000000, 4.500000000000000000, -118.0000000000000284 ) ) ;
#1861 = CARTESIAN_POINT ( 'NONE',  ( -114.9999999999999716, 114.9999999999999858, 20.00000000000000000 ) ) ;
#1862 = ORIENTED_EDGE ( 'NONE', *, *, #6074, .F. ) ;
#1863 = ITEM_DEFINED_TRANSFORMATION ( 'NONE', 'NONE', #6643,  #1299 ) ;
#1864 = VECTOR ( 'NONE', #5763, 1000.000000000000000 ) ;
#1865 = CARTESIAN_POINT ( 'NONE',  ( 7.630101673356683101, 49.41909675622682840, -22.43442449636368252 ) ) ;
#1866 = EDGE_CURVE ( 'NONE', #6494, #167, #4693, .T. ) ;
#1867 = EDGE_CURVE ( 'NONE', #8175, #3044, #4291, .T. ) ;
#1868 = EDGE_CURVE ( 'NONE', #5616, #5480, #4408, .T. ) ;
#1869 = PRESENTATION_LAYER_ASSIGNMENT (  '', '', ( #1309 ) ) ;
#1870 = ORIENTED_EDGE ( 'NONE', *, *, #937, .T. ) ;
#1871 = VECTOR ( 'NONE', #1719, 1000.000000000000000 ) ;
#1872 = CARTESIAN_POINT ( 'NONE',  ( 120.0000000000000000, -115.0000000000000000, 340.0000000000000000 ) ) ;
#1873 = AXIS2_PLACEMENT_3D ( 'NONE', #7567, #1735, #7517 ) ;
#1874 = EDGE_LOOP ( 'NONE', ( #1791, #8170, #4052, #6913 ) ) ;
#1875 = LINE ( 'NONE', #5150, #6737 ) ;
#1876 = CYLINDRICAL_SURFACE ( 'NONE', #1814, 15.00000000000000000 ) ;
#1877 = AXIS2_PLACEMENT_3D ( 'NONE', #1596, #5896, #7892 ) ;
#1878 = VERTEX_POINT ( 'NONE', #6800 ) ;
#1879 = CARTESIAN_POINT ( 'NONE',  ( -6.260380647299085055, 49.60786550102537973, -23.32709356835263748 ) ) ;
#1880 = ADVANCED_FACE ( 'NONE', ( #948 ), #2153, .F. ) ;
#1881 = CIRCLE ( 'NONE', #1333, 2.499999999999984013 ) ;
#1882 = PLANE ( 'NONE',  #1572 ) ;
#1883 = EDGE_LOOP ( 'NONE', ( #3663, #1360, #5279, #4808 ) ) ;
#1884 = CIRCLE ( 'NONE', #2423, 12.49999999999999289 ) ;
#1885 = DIRECTION ( 'NONE',  ( -0.000000000000000000, -1.000000000000000000, -0.000000000000000000 ) ) ;
#1886 = CARTESIAN_POINT ( 'NONE',  ( 0.000000000000000000, 0.000000000000000000, -126.0000000000000284 ) ) ;
#1887 = CIRCLE ( 'NONE', #1471, 8.999999999999994671 ) ;
#1888 = CARTESIAN_POINT ( 'NONE',  ( 0.000000000000000000, -1.262567713204993255E-33, -150.0000000000000000 ) ) ;
#1889 = VERTEX_POINT ( 'NONE', #2953 ) ;
#1890 = CARTESIAN_POINT ( 'NONE',  ( -10.16275934324372265, -48.95683464664497819, -19.78926114801198821 ) ) ;
#1891 = ORIENTED_EDGE ( 'NONE', *, *, #7608, .F. ) ;
#1892 = AXIS2_PLACEMENT_3D ( 'NONE', #4105, #7499, #5471 ) ;
#1893 = CIRCLE ( 'NONE', #2163, 4.999999999999990230 ) ;
#1894 = DIRECTION ( 'NONE',  ( -0.000000000000000000, -0.000000000000000000, -1.000000000000000000 ) ) ;
#1895 = CYLINDRICAL_SURFACE ( 'NONE', #4148, 37.49999999999999289 ) ;
#1896 = CARTESIAN_POINT ( 'NONE',  ( 12.07731880710695904, -48.51961889015784379, -15.74894529186713577 ) ) ;
#1897 = VECTOR ( 'NONE', #1280, 1000.000000000000000 ) ;
#1898 = DIRECTION ( 'NONE',  ( -0.000000000000000000, -0.000000000000000000, 1.000000000000000000 ) ) ;
#1899 = PRESENTATION_LAYER_ASSIGNMENT (  '', '', ( #7953 ) ) ;
#1900 = DIRECTION ( 'NONE',  ( 0.000000000000000000, 0.000000000000000000, -1.000000000000000000 ) ) ;
#1901 = ORIENTED_EDGE ( 'NONE', *, *, #6845, .T. ) ;
#1902 = VECTOR ( 'NONE', #2179, 1000.000000000000000 ) ;
#1903 = CARTESIAN_POINT ( 'NONE',  ( -114.9999999999999858, -114.9999999999999858, 10.00000000000000000 ) ) ;
#1904 = VERTEX_POINT ( 'NONE', #7572 ) ;
#1905 = CARTESIAN_POINT ( 'NONE',  ( 10.40000000000000036, 0.000000000000000000, 0.000000000000000000 ) ) ;
#1906 = ORIENTED_EDGE ( 'NONE', *, *, #2484, .T. ) ;
#1907 = EDGE_CURVE ( 'NONE', #5704, #1427, #8347, .T. ) ;
#1908 = DIRECTION ( 'NONE',  ( 1.000000000000000000, 0.000000000000000000, 0.000000000000000000 ) ) ;
#1909 = DIRECTION ( 'NONE',  ( 1.000000000000000000, 0.000000000000000000, 0.000000000000000000 ) ) ;
#1910 = CONTEXT_DEPENDENT_SHAPE_REPRESENTATION ( #4071, #8307 ) ;
#1911 = ORIENTED_EDGE ( 'NONE', *, *, #7216, .T. ) ;
#1912 = CARTESIAN_POINT ( 'NONE',  ( 0.4088724290315675081, 49.99999999999999289, -24.99999999999999645 ) ) ;
#1913 = VECTOR ( 'NONE', #8057, 1000.000000000000000 ) ;
#1914 = ORIENTED_EDGE ( 'NONE', *, *, #5462, .F. ) ;
#1915 = EDGE_CURVE ( 'NONE', #6329, #6306, #3408, .T. ) ;
#1916 = ORIENTED_EDGE ( 'NONE', *, *, #5562, .T. ) ;
#1917 = CARTESIAN_POINT ( 'NONE',  ( -7.743805596760466869E-14, -12.50000000000000888, 54.99999999999997868 ) ) ;
#1918 = VERTEX_POINT ( 'NONE', #7219 ) ;
#1919 = ADVANCED_FACE ( 'NONE', ( #2008 ), #5194, .T. ) ;
#1920 = DIRECTION ( 'NONE',  ( 1.000000000000000000, 0.000000000000000000, 0.000000000000000000 ) ) ;
#1921 = EDGE_CURVE ( 'NONE', #67, #5909, #2099, .T. ) ;
#1922 = ADVANCED_FACE ( 'NONE', ( #2703, #5284 ), #890, .F. ) ;
#1923 = CARTESIAN_POINT ( 'NONE',  ( -9.123515037571456432, 49.16144051280856786, -21.05438506594878945 ) ) ;
#1924 = DIRECTION ( 'NONE',  ( -1.000000000000000000, 0.000000000000000000, -0.000000000000000000 ) ) ;
#1925 = CARTESIAN_POINT ( 'NONE',  ( 17.61817604250836311, 4.500000000000000000, -120.5000000000000284 ) ) ;
#1926 = ORIENTED_EDGE ( 'NONE', *, *, #1235, .F. ) ;
#1927 = VECTOR ( 'NONE', #2123, 1000.000000000000000 ) ;
#1928 = DIRECTION ( 'NONE',  ( 1.000000000000000000, 0.000000000000000000, 0.000000000000000000 ) ) ;
#1929 = DIRECTION ( 'NONE',  ( -0.000000000000000000, 0.000000000000000000, 1.000000000000000000 ) ) ;
#1930 = ADVANCED_FACE ( 'NONE', ( #7832 ), #6986, .T. ) ;
#1931 = PLANE ( 'NONE',  #7835 ) ;
#1932 = EDGE_LOOP ( 'NONE', ( #5556, #4034 ) ) ;
#1933 = CARTESIAN_POINT ( 'NONE',  ( 5.000000000000000000, -4.685197434473809430, 7.372574772901430151E-15 ) ) ;
#1934 = SHAPE_REPRESENTATION_RELATIONSHIP ( 'NONE' , 'NONE' ,  #4267, #1400 ) ;
#1935 = VERTEX_POINT ( 'NONE', #5949 ) ;
#1936 = CIRCLE ( 'NONE', #713, 54.99999999999995026 ) ;
#1937 = DIRECTION ( 'NONE',  ( 0.000000000000000000, 1.000000000000000000, 0.000000000000000000 ) ) ;
#1938 = EDGE_CURVE ( 'NONE', #5315, #1010, #2286, .T. ) ;
#1939 = LINE ( 'NONE', #1808, #6729 ) ;
#1940 = CARTESIAN_POINT ( 'NONE',  ( 115.0000000000000284, -115.0000000000000000, 70.00000000000000000 ) ) ;
#1941 = CARTESIAN_POINT ( 'NONE',  ( 10.40000000000000036, 0.000000000000000000, 5.000000000000035527 ) ) ;
#1942 = AXIS2_PLACEMENT_3D ( 'NONE', #4989, #5072, #604 ) ;
#1943 = DIRECTION ( 'NONE',  ( 0.000000000000000000, -1.000000000000000000, -2.960594732333750117E-16 ) ) ;
#1944 = AXIS2_PLACEMENT_3D ( 'NONE', #933, #5442, #7189 ) ;
#1945 = PLANE ( 'NONE',  #88 ) ;
#1946 = VERTEX_POINT ( 'NONE', #4719 ) ;
#1947 = CARTESIAN_POINT ( 'NONE',  ( 0.000000000000000000, -125.0000000000000000, -12.50000000000000000 ) ) ;
#1948 = ORIENTED_EDGE ( 'NONE', *, *, #885, .F. ) ;
#1949 = ORIENTED_EDGE ( 'NONE', *, *, #8105, .F. ) ;
#1950 = CARTESIAN_POINT ( 'NONE',  ( -50.00000000000000711, -55.00000000000000000, 220.0000000000000284 ) ) ;
#1951 = EDGE_LOOP ( 'NONE', ( #3758, #5816, #825, #2312 ) ) ;
#1952 = DIRECTION ( 'NONE',  ( 0.000000000000000000, 2.960594732333750610E-16, -1.000000000000000000 ) ) ;
#1953 = CARTESIAN_POINT ( 'NONE',  ( 1.592040838891559490E-15, 125.0000000000000568, 92.99999999999992895 ) ) ;
#1954 = CARTESIAN_POINT ( 'NONE',  ( -104.9999999999999432, -105.0000000000000853, 240.0000000000000284 ) ) ;
#1955 = CONTEXT_DEPENDENT_SHAPE_REPRESENTATION ( #6671, #5741 ) ;
#1956 = ORIENTED_EDGE ( 'NONE', *, *, #7898, .T. ) ;
#1957 = CARTESIAN_POINT ( 'NONE',  ( 12.50034226774477730, 48.41220345444930473, -13.31371842734950839 ) ) ;
#1958 = AXIS2_PLACEMENT_3D ( 'NONE', #7833, #3321, #2667 ) ;
#1959 = ORIENTED_EDGE ( 'NONE', *, *, #2080, .T. ) ;
#1960 = CARTESIAN_POINT ( 'NONE',  ( 59.99999999999999289, -55.00000000000000000, 220.0000000000000284 ) ) ;
#1961 = CYLINDRICAL_SURFACE ( 'NONE', #4815, 4.999999999999990230 ) ;
#1962 = VERTEX_POINT ( 'NONE', #3358 ) ;
#1963 = ORIENTED_EDGE ( 'NONE', *, *, #4837, .F. ) ;
#1964 = DIRECTION ( 'NONE',  ( 1.000000000000000000, 0.000000000000000000, 0.000000000000000000 ) ) ;
#1965 = CARTESIAN_POINT ( 'NONE',  ( -120.0000000000000000, 115.0000000000000000, 270.0000000000000000 ) ) ;
#1966 = EDGE_CURVE ( 'NONE', #2083, #8025, #7305, .T. ) ;
#1967 = ORIENTED_EDGE ( 'NONE', *, *, #949, .T. ) ;
#1968 = EDGE_CURVE ( 'NONE', #6651, #8339, #1884, .T. ) ;
#1969 = DIRECTION ( 'NONE',  ( 0.000000000000000000, 0.000000000000000000, 1.000000000000000000 ) ) ;
#1970 = CARTESIAN_POINT ( 'NONE',  ( 54.99999999999999289, -55.00000000000000711, -27.50000000000000000 ) ) ;
#1971 = LINE ( 'NONE', #3126, #6847 ) ;
#1972 = CARTESIAN_POINT ( 'NONE',  ( 0.000000000000000000, -72.49999999999994316, -212.5000000000000568 ) ) ;
#1973 = CARTESIAN_POINT ( 'NONE',  ( -49.00000000000000000, 55.00000000000000711, 27.50000000000000000 ) ) ;
#1974 = ORIENTED_EDGE ( 'NONE', *, *, #2868, .T. ) ;
#1975 = CARTESIAN_POINT ( 'NONE',  ( -8.257771144136533792, -49.31688802671483529, -21.91964719072836232 ) ) ;
#1976 = EDGE_CURVE ( 'NONE', #66, #5533, #7130, .T. ) ;
#1977 =( NAMED_UNIT ( * ) SI_UNIT ( $, .STERADIAN. ) SOLID_ANGLE_UNIT ( ) );
#1978 = ORIENTED_EDGE ( 'NONE', *, *, #1026, .F. ) ;
#1979 = FACE_OUTER_BOUND ( 'NONE', #608, .T. ) ;
#1980 = EDGE_CURVE ( 'NONE', #7524, #2265, #2627, .T. ) ;
#1981 = VECTOR ( 'NONE', #4658, 1000.000000000000000 ) ;
#1982 = LINE ( 'NONE', #90, #3734 ) ;
#1983 = DIRECTION ( 'NONE',  ( 0.000000000000000000, 0.000000000000000000, 1.000000000000000000 ) ) ;
#1984 = CARTESIAN_POINT ( 'NONE',  ( 5.000000000000000000, 2.342598717236902939, -4.057500000000001883 ) ) ;
#1985 = CARTESIAN_POINT ( 'NONE',  ( -54.99999999999999289, 55.00000000000000711, -27.50000000000000000 ) ) ;
#1986 = PRODUCT_DEFINITION_SHAPE ( 'NONE', 'NONE',  #8357 ) ;
#1987 = DIRECTION ( 'NONE',  ( -1.000000000000000000, 0.000000000000000000, -0.000000000000000000 ) ) ;
#1988 = EDGE_CURVE ( 'NONE', #1680, #6868, #7261, .T. ) ;
#1989 = ORIENTED_EDGE ( 'NONE', *, *, #4023, .T. ) ;
#1990 = EDGE_CURVE ( 'NONE', #4182, #4386, #8216, .T. ) ;
#1991 = FACE_OUTER_BOUND ( 'NONE', #5640, .T. ) ;
#1992 = ORIENTED_EDGE ( 'NONE', *, *, #5607, .F. ) ;
#1993 = CIRCLE ( 'NONE', #3040, 25.00000000000000000 ) ;
#1994 = ORIENTED_EDGE ( 'NONE', *, *, #2474, .T. ) ;
#1995 = CARTESIAN_POINT ( 'NONE',  ( 125.0000000000000000, -52.50000000000000000, 190.0000000000000284 ) ) ;
#1996 = CIRCLE ( 'NONE', #3715, 12.50000000000000000 ) ;
#1997 = ORIENTED_EDGE ( 'NONE', *, *, #2026, .T. ) ;
#1998 = LINE ( 'NONE', #7601, #376 ) ;
#1999 = LINE ( 'NONE', #4491, #3203 ) ;
#2000 = CARTESIAN_POINT ( 'NONE',  ( -54.99999999999999289, 55.00000000000000711, -27.50000000000000000 ) ) ;
#2001 = CONTEXT_DEPENDENT_SHAPE_REPRESENTATION ( #7382, #7848 ) ;
#2002 = DIRECTION ( 'NONE',  ( 0.000000000000000000, -0.4999999999999984457, 0.8660254037844394848 ) ) ;
#2003 = MECHANICAL_DESIGN_GEOMETRIC_PRESENTATION_REPRESENTATION (  '', ( #5880 ), #488 ) ;
#2004 = CARTESIAN_POINT ( 'NONE',  ( 55.00000000000000000, 55.00000000000000000, 220.0000000000000284 ) ) ;
#2005 = CARTESIAN_POINT ( 'NONE',  ( 121.0000000000000284, -115.0000000000000000, 70.00000000000000000 ) ) ;
#2006 = ORIENTED_EDGE ( 'NONE', *, *, #8312, .F. ) ;
#2007 = AXIS2_PLACEMENT_3D ( 'NONE', #7496, #7627, #6901 ) ;
#2008 = FACE_OUTER_BOUND ( 'NONE', #8041, .T. ) ;
#2009 = DIRECTION ( 'NONE',  ( 0.000000000000000000, 1.000000000000000000, 0.000000000000000000 ) ) ;
#2010 = AXIS2_PLACEMENT_3D ( 'NONE', #7360, #7954, #8028 ) ;
#2011 = FACE_BOUND ( 'NONE', #2386, .T. ) ;
#2012 = CARTESIAN_POINT ( 'NONE',  ( 105.0000000000000000, 72.49999999999994316, 240.0000000000000284 ) ) ;
#2013 = DIRECTION ( 'NONE',  ( 6.106226635438364917E-16, 3.154042683594196846E-17, 1.000000000000000000 ) ) ;
#2014 = CIRCLE ( 'NONE', #6979, 12.99999999999999822 ) ;
#2015 = CARTESIAN_POINT ( 'NONE',  ( 95.00000000000002842, -95.00000000000002842, 70.00000000000000000 ) ) ;
#2016 = DIRECTION ( 'NONE',  ( 1.000000000000000000, 0.000000000000000000, 0.000000000000000000 ) ) ;
#2017 = DIRECTION ( 'NONE',  ( -1.000000000000000000, -0.000000000000000000, -0.000000000000000000 ) ) ;
#2018 = ADVANCED_FACE ( 'NONE', ( #4678, #7262 ), #1482, .F. ) ;
#2019 = VERTEX_POINT ( 'NONE', #3396 ) ;
#2020 = DIRECTION ( 'NONE',  ( -0.8571673007021134438, 1.049727191138620051E-16, 0.5150380749100522682 ) ) ;
#2021 = DIRECTION ( 'NONE',  ( 7.216449660063517513E-16, 1.000000000000000000, 2.218671295934102709E-31 ) ) ;
#2022 = EDGE_LOOP ( 'NONE', ( #6636, #1140, #3559, #3514 ) ) ;
#2023 = TOROIDAL_SURFACE ( 'NONE', #3455, 5.400000000000035882, 0.4000000000000000222 ) ;
#2024 = ORIENTED_EDGE ( 'NONE', *, *, #4512, .F. ) ;
#2025 = FACE_OUTER_BOUND ( 'NONE', #7078, .T. ) ;
#2026 = EDGE_CURVE ( 'NONE', #6580, #5343, #5986, .T. ) ;
#2027 = AXIS2_PLACEMENT_3D ( 'NONE', #3385, #5895, #2157 ) ;
#2028 = AXIS2_PLACEMENT_3D ( 'NONE', #8099, #3603, #7469 ) ;
#2029 = FACE_OUTER_BOUND ( 'NONE', #6543, .T. ) ;
#2030 = ADVANCED_FACE ( 'NONE', ( #415 ), #8104, .T. ) ;
#2031 = AXIS2_PLACEMENT_3D ( 'NONE', #2189, #4740, #7321 ) ;
#2032 = EDGE_CURVE ( 'NONE', #6276, #1109, #7478, .T. ) ;
#2033 = SURFACE_STYLE_FILL_AREA ( #1419 ) ;
#2034 = EDGE_CURVE ( 'NONE', #6639, #2500, #5444, .T. ) ;
#2035 = CARTESIAN_POINT ( 'NONE',  ( -105.0000000000000000, 72.49999999999994316, 240.0000000000000284 ) ) ;
#2036 = AXIS2_PLACEMENT_3D ( 'NONE', #964, #6773, #2282 ) ;
#2037 = AXIS2_PLACEMENT_3D ( 'NONE', #3347, #2118, #2154 ) ;
#2038 = FACE_OUTER_BOUND ( 'NONE', #3344, .T. ) ;
#2039 = ORIENTED_EDGE ( 'NONE', *, *, #5463, .T. ) ;
#2040 = VERTEX_POINT ( 'NONE', #8147 ) ;
#2041 = VERTEX_POINT ( 'NONE', #6787 ) ;
#2042 = FACE_OUTER_BOUND ( 'NONE', #6018, .T. ) ;
#2043 = VECTOR ( 'NONE', #2971, 1000.000000000000000 ) ;
#2044 = VECTOR ( 'NONE', #3445, 1000.000000000000000 ) ;
#2045 = EDGE_LOOP ( 'NONE', ( #1633, #379, #4234, #5708 ) ) ;
#2046 = DIRECTION ( 'NONE',  ( 0.000000000000000000, 0.000000000000000000, -1.000000000000000000 ) ) ;
#2047 = CARTESIAN_POINT ( 'NONE',  ( -60.99999999999998579, -55.00000000000000711, 27.50000000000000000 ) ) ;
#2048 = VERTEX_POINT ( 'NONE', #6067 ) ;
#2049 = CARTESIAN_POINT ( 'NONE',  ( 55.00000000000000000, -55.00000000000000000, 240.0000000000000284 ) ) ;
#2050 = VECTOR ( 'NONE', #7364, 1000.000000000000000 ) ;
#2051 = EDGE_LOOP ( 'NONE', ( #4977, #6871 ) ) ;
#2052 = ORIENTED_EDGE ( 'NONE', *, *, #6603, .T. ) ;
#2053 = DIRECTION ( 'NONE',  ( -1.000000000000000000, -0.000000000000000000, -0.000000000000000000 ) ) ;
#2054 = ORIENTED_EDGE ( 'NONE', *, *, #2757, .F. ) ;
#2055 = DIRECTION ( 'NONE',  ( -1.000000000000000000, 0.000000000000000000, 0.000000000000000000 ) ) ;
#2056 = EDGE_CURVE ( 'NONE', #8025, #1889, #4282, .T. ) ;
#2057 = ORIENTED_EDGE ( 'NONE', *, *, #4536, .F. ) ;
#2058 = DIRECTION ( 'NONE',  ( -0.000000000000000000, -0.000000000000000000, -1.000000000000000000 ) ) ;
#2059 = FACE_OUTER_BOUND ( 'NONE', #4783, .T. ) ;
#2060 = ORIENTED_EDGE ( 'NONE', *, *, #6540, .T. ) ;
#2061 = CARTESIAN_POINT ( 'NONE',  ( 9.999999999999994671, 0.000000000000000000, 8.000000000000000000 ) ) ;
#2062 = DIRECTION ( 'NONE',  ( -1.752490724247359037E-17, 1.000000000000000000, 3.853078496550133260E-17 ) ) ;
#2063 = DIRECTION ( 'NONE',  ( -0.000000000000000000, -0.000000000000000000, 1.000000000000000000 ) ) ;
#2064 = PRODUCT_DEFINITION_SHAPE ( 'NONE', 'NONE',  #557 ) ;
#2065 = LINE ( 'NONE', #3366, #3354 ) ;
#2066 = ORIENTED_EDGE ( 'NONE', *, *, #7515, .F. ) ;
#2067 = CARTESIAN_POINT ( 'NONE',  ( -120.0000000000000000, -115.0000000000000000, 340.0000000000000000 ) ) ;
#2068 = DIRECTION ( 'NONE',  ( 1.000000000000000000, 3.155443620884047222E-30, 1.224646799147346798E-16 ) ) ;
#2069 =( REPRESENTATION_RELATIONSHIP ('NONE','NONE', #6882, #4267 ) REPRESENTATION_RELATIONSHIP_WITH_TRANSFORMATION ( #7693 )SHAPE_REPRESENTATION_RELATIONSHIP( ) );
#2070 = CARTESIAN_POINT ( 'NONE',  ( 114.9999999999999147, -115.0000000000000000, 8.205133554287239938E-16 ) ) ;
#2071 = EDGE_LOOP ( 'NONE', ( #4525, #6589, #7855 ) ) ;
#2072 = CARTESIAN_POINT ( 'NONE',  ( -125.0000000000000000, 52.50000000000000000, 190.0000000000000284 ) ) ;
#2073 = DIRECTION ( 'NONE',  ( 0.000000000000000000, 1.000000000000000000, 0.000000000000000000 ) ) ;
#2074 = CARTESIAN_POINT ( 'NONE',  ( 125.0000000000000000, -52.49999999999997158, 0.000000000000000000 ) ) ;
#2075 = FILL_AREA_STYLE_COLOUR ( '', #5074 ) ;
#2076 = CARTESIAN_POINT ( 'NONE',  ( 75.00000000000000000, 0.000000000000000000, 0.000000000000000000 ) ) ;
#2077 = PRODUCT_RELATED_PRODUCT_CATEGORY ( 'part', '', ( #6807 ) ) ;
#2078 = ORIENTED_EDGE ( 'NONE', *, *, #8225, .F. ) ;
#2079 = EDGE_CURVE ( 'NONE', #4329, #3292, #4168, .T. ) ;
#2080 = EDGE_CURVE ( 'NONE', #3696, #2372, #2373, .T. ) ;
#2081 = EDGE_LOOP ( 'NONE', ( #147, #6748, #1034, #3870, #55, #6533, #2869, #3571 ) ) ;
#2082 = FACE_OUTER_BOUND ( 'NONE', #561, .T. ) ;
#2083 = VERTEX_POINT ( 'NONE', #1567 ) ;
#2084 = CARTESIAN_POINT ( 'NONE',  ( 80.00000000000000000, 4.171999999999999709, 0.000000000000000000 ) ) ;
#2085 = AXIS2_PLACEMENT_3D ( 'NONE', #5602, #445, #663 ) ;
#2086 = LINE ( 'NONE', #916, #3884 ) ;
#2087 = DIRECTION ( 'NONE',  ( 0.8571673007021134438, 0.000000000000000000, 0.5150380749100522682 ) ) ;
#2088 = EDGE_CURVE ( 'NONE', #2457, #5057, #5401, .T. ) ;
#2089 = EDGE_LOOP ( 'NONE', ( #2586, #7609 ) ) ;
#2090 = AXIS2_PLACEMENT_3D ( 'NONE', #4600, #2777, #1319 ) ;
#2091 = ADVANCED_FACE ( 'NONE', ( #2215 ), #6199, .T. ) ;
#2092 =( GEOMETRIC_REPRESENTATION_CONTEXT ( 3 ) GLOBAL_UNCERTAINTY_ASSIGNED_CONTEXT ( ( #4446 ) ) GLOBAL_UNIT_ASSIGNED_CONTEXT ( ( #5803, #7719, #1977 ) ) REPRESENTATION_CONTEXT ( 'NONE', 'WORKASPACE' ) );
#2093 = CARTESIAN_POINT ( 'NONE',  ( 125.0000000000000000, -125.0000000000000284, 70.00000000000000000 ) ) ;
#2094 = DIRECTION ( 'NONE',  ( -0.000000000000000000, -0.000000000000000000, 1.000000000000000000 ) ) ;
#2095 = ORIENTED_EDGE ( 'NONE', *, *, #6647, .T. ) ;
#2096 = SURFACE_STYLE_FILL_AREA ( #806 ) ;
#2097 = VERTEX_POINT ( 'NONE', #1610 ) ;
#2098 = AXIS2_PLACEMENT_3D ( 'NONE', #4174, #6763, #5459 ) ;
#2099 = LINE ( 'NONE', #726, #1736 ) ;
#2100 = EDGE_CURVE ( 'NONE', #469, #8240, #4120, .T. ) ;
#2101 = CIRCLE ( 'NONE', #4632, 12.99999999999999822 ) ;
#2102 = DIRECTION ( 'NONE',  ( -0.000000000000000000, -0.000000000000000000, 1.000000000000000000 ) ) ;
#2103 = CARTESIAN_POINT ( 'NONE',  ( -125.0000000000002558, -125.0000000000000000, 20.00000000000000000 ) ) ;
#2104 = LINE ( 'NONE', #5410, #2044 ) ;
#2105 = EDGE_CURVE ( 'NONE', #5395, #2109, #556, .T. ) ;
#2106 = CARTESIAN_POINT ( 'NONE',  ( -55.00000000000000000, 55.00000000000000000, 240.0000000000000284 ) ) ;
#2107 = ORIENTED_EDGE ( 'NONE', *, *, #1564, .T. ) ;
#2108 = CARTESIAN_POINT ( 'NONE',  ( 0.000000000000000000, 0.000000000000000000, -118.0000000000000284 ) ) ;
#2109 = VERTEX_POINT ( 'NONE', #2259 ) ;
#2110 = CARTESIAN_POINT ( 'NONE',  ( -60.99999999999997868, 55.00000000000000711, -27.50000000000000000 ) ) ;
#2111=STYLED_ITEM('',(#8386),#826);
#2112 = PRODUCT_DEFINITION_SHAPE ( 'NONE', 'NONE',  #6949 ) ;
#2113 = CARTESIAN_POINT ( 'NONE',  ( -104.9999999999999432, -105.0000000000000853, 240.0000000000000284 ) ) ;
#2114 = LINE ( 'NONE', #4656, #1435 ) ;
#2115 = CARTESIAN_POINT ( 'NONE',  ( 79.17200000000011073, 6.123233995736852071E-16, -5.000000000000070166 ) ) ;
#2116 = ORIENTED_EDGE ( 'NONE', *, *, #4902, .F. ) ;
#2117 = DIRECTION ( 'NONE',  ( 0.000000000000000000, 0.000000000000000000, 1.000000000000000000 ) ) ;
#2118 = DIRECTION ( 'NONE',  ( -0.000000000000000000, -7.945337353457666666E-18, -1.000000000000000000 ) ) ;
#2119 = ORIENTED_EDGE ( 'NONE', *, *, #2298, .T. ) ;
#2120 = DIRECTION ( 'NONE',  ( -0.000000000000000000, -0.000000000000000000, 1.000000000000000000 ) ) ;
#2121 = LINE ( 'NONE', #4668, #5089 ) ;
#2122 = ADVANCED_FACE ( 'NONE', ( #6834 ), #5407, .F. ) ;
#2123 = DIRECTION ( 'NONE',  ( 0.000000000000000000, 1.000000000000000000, 0.000000000000000000 ) ) ;
#2124 = AXIS2_PLACEMENT_3D ( 'NONE', #6427, #3220, #2606 ) ;
#2125 = EDGE_LOOP ( 'NONE', ( #7392, #3168, #5494, #5366 ) ) ;
#2126 = DIRECTION ( 'NONE',  ( -1.000000000000000000, -0.000000000000000000, -0.000000000000000000 ) ) ;
#2127 = CIRCLE ( 'NONE', #6821, 4.999999999999997335 ) ;
#2128 = ORIENTED_EDGE ( 'NONE', *, *, #5048, .F. ) ;
#2129 = DIRECTION ( 'NONE',  ( 1.000000000000000000, 0.000000000000000000, 0.000000000000000000 ) ) ;
#2130 = EDGE_CURVE ( 'NONE', #6306, #6329, #5453, .T. ) ;
#2131 = VECTOR ( 'NONE', #8255, 1000.000000000000000 ) ;
#2132 = CARTESIAN_POINT ( 'NONE',  ( 0.000000000000000000, 0.000000000000000000, -28.00000000000002487 ) ) ;
#2133 = DIRECTION ( 'NONE',  ( 1.000000000000000000, 0.000000000000000000, 0.000000000000000000 ) ) ;
#2134 = AXIS2_PLACEMENT_3D ( 'NONE', #8300, #6470, #614 ) ;
#2135 = FACE_OUTER_BOUND ( 'NONE', #1820, .T. ) ;
#2136 = CARTESIAN_POINT ( 'NONE',  ( 5.000000000000000000, 4.685197434473814759, -5.637851296924623057E-15 ) ) ;
#2137 = FACE_OUTER_BOUND ( 'NONE', #8280, .T. ) ;
#2138 = DIRECTION ( 'NONE',  ( 1.000000000000000000, 0.000000000000000000, 0.000000000000000000 ) ) ;
#2139 = ORIENTED_EDGE ( 'NONE', *, *, #1702, .T. ) ;
#2140 = CYLINDRICAL_SURFACE ( 'NONE', #5625, 25.00000000000000000 ) ;
#2141 = EDGE_CURVE ( 'NONE', #4379, #1618, #7164, .T. ) ;
#2142 = DIRECTION ( 'NONE',  ( 1.000000000000000000, 0.000000000000000000, 0.000000000000000000 ) ) ;
#2143 = CARTESIAN_POINT ( 'NONE',  ( 0.000000000000000000, 0.000000000000000000, -250.0000000000000000 ) ) ;
#2144 = VECTOR ( 'NONE', #28, 1000.000000000000000 ) ;
#2145 = DIRECTION ( 'NONE',  ( 0.000000000000000000, 0.000000000000000000, -1.000000000000000000 ) ) ;
#2146 =( NAMED_UNIT ( * ) SI_UNIT ( $, .STERADIAN. ) SOLID_ANGLE_UNIT ( ) );
#2147 = SHAPE_REPRESENTATION_RELATIONSHIP ( 'NONE' , 'NONE' ,  #2264, #594 ) ;
#2148 = LINE ( 'NONE', #7288, #4364 ) ;
#2149 = CARTESIAN_POINT ( 'NONE',  ( 120.5000000000000000, -114.9999999999999716, 20.00000000000000000 ) ) ;
#2150 = ORIENTED_EDGE ( 'NONE', *, *, #1542, .F. ) ;
#2151 = VECTOR ( 'NONE', #7134, 1000.000000000000000 ) ;
#2152 = CARTESIAN_POINT ( 'NONE',  ( 120.0000000000000000, -125.0000000000000000, -28.00000000000002487 ) ) ;
#2153 = CONICAL_SURFACE ( 'NONE', #6444, 5.999999999999991118, 1.029744258676652313 ) ;
#2154 = DIRECTION ( 'NONE',  ( 0.000000000000000000, 1.000000000000000000, -7.945337353457666666E-18 ) ) ;
#2155 = FACE_OUTER_BOUND ( 'NONE', #1496, .T. ) ;
#2156 = ORIENTED_EDGE ( 'NONE', *, *, #4836, .T. ) ;
#2157 = DIRECTION ( 'NONE',  ( 0.000000000000000000, 0.000000000000000000, -1.000000000000000000 ) ) ;
#2158 = DIRECTION ( 'NONE',  ( -0.000000000000000000, -0.000000000000000000, 1.000000000000000000 ) ) ;
#2159 = VECTOR ( 'NONE', #4968, 1000.000000000000000 ) ;
#2160 = VECTOR ( 'NONE', #1857, 1000.000000000000000 ) ;
#2161 = ORIENTED_EDGE ( 'NONE', *, *, #3332, .T. ) ;
#2162 = AXIS2_PLACEMENT_3D ( 'NONE', #53, #5882, #7285 ) ;
#2163 = AXIS2_PLACEMENT_3D ( 'NONE', #528, #8221, #1168 ) ;
#2164 = EDGE_CURVE ( 'NONE', #6732, #509, #7739, .T. ) ;
#2165 = ORIENTED_EDGE ( 'NONE', *, *, #1564, .F. ) ;
#2166 = DIRECTION ( 'NONE',  ( 0.000000000000000000, 0.000000000000000000, 1.000000000000000000 ) ) ;
#2167 = ORIENTED_EDGE ( 'NONE', *, *, #4580, .T. ) ;
#2168 = FILL_AREA_STYLE_COLOUR ( '', #6189 ) ;
#2169 = AXIS2_PLACEMENT_3D ( 'NONE', #4286, #3713, #6244 ) ;
#2170 = CARTESIAN_POINT ( 'NONE',  ( 120.0000000000000000, 120.0000000000000000, -28.00000000000002487 ) ) ;
#2171 = ADVANCED_FACE ( 'NONE', ( #4410 ), #1231, .T. ) ;
#2172 = EDGE_CURVE ( 'NONE', #1878, #7656, #1103, .T. ) ;
#2173 = CARTESIAN_POINT ( 'NONE',  ( 60.00000000000000000, 55.00000000000000000, 240.0000000000000284 ) ) ;
#2174 = EDGE_CURVE ( 'NONE', #4652, #293, #4596, .T. ) ;
#2175 = AXIS2_PLACEMENT_3D ( 'NONE', #1726, #1575, #3608 ) ;
#2176 = DIRECTION ( 'NONE',  ( 0.000000000000000000, 0.000000000000000000, -1.000000000000000000 ) ) ;
#2177 = CARTESIAN_POINT ( 'NONE',  ( -115.0000000000000000, 115.0000000000000000, 270.0000000000000000 ) ) ;
#2178 = DIRECTION ( 'NONE',  ( -1.000000000000000000, -0.000000000000000000, -0.000000000000000000 ) ) ;
#2179 = DIRECTION ( 'NONE',  ( 1.000000000000000000, 0.000000000000000000, 0.000000000000000000 ) ) ;
#2180 = EDGE_LOOP ( 'NONE', ( #2394, #6230 ) ) ;
#2181 = CARTESIAN_POINT ( 'NONE',  ( 115.0000000000000284, -115.0000000000000000, 20.00000000000000355 ) ) ;
#2182 = ORIENTED_EDGE ( 'NONE', *, *, #3572, .F. ) ;
#2183 = EDGE_CURVE ( 'NONE', #2571, #5439, #5014, .T. ) ;
#2184 = EDGE_CURVE ( 'NONE', #5018, #7120, #6621, .T. ) ;
#2185 = DIRECTION ( 'NONE',  ( -0.000000000000000000, -1.000000000000000000, -0.000000000000000000 ) ) ;
#2186 = EDGE_CURVE ( 'NONE', #4012, #5626, #5543, .T. ) ;
#2187 = DIRECTION ( 'NONE',  ( -0.000000000000000000, -0.000000000000000000, -1.000000000000000000 ) ) ;
#2188 = DIRECTION ( 'NONE',  ( -1.000000000000000000, -0.000000000000000000, -0.000000000000000000 ) ) ;
#2189 = CARTESIAN_POINT ( 'NONE',  ( -115.0000000000000000, 115.0000000000000000, 270.0000000000000000 ) ) ;
#2190 = VECTOR ( 'NONE', #366, 1000.000000000000000 ) ;
#2191 = CARTESIAN_POINT ( 'NONE',  ( 0.000000000000000000, 0.000000000000000000, 0.000000000000000000 ) ) ;
#2192 = CARTESIAN_POINT ( 'NONE',  ( 0.000000000000000000, -115.0000000000000000, 250.0000000000000000 ) ) ;
#2193 = CARTESIAN_POINT ( 'NONE',  ( 105.0000000000000000, -105.0000000000000568, 240.0000000000000284 ) ) ;
#2194 = ORIENTED_EDGE ( 'NONE', *, *, #6340, .T. ) ;
#2195 = DIRECTION ( 'NONE',  ( -0.000000000000000000, -0.000000000000000000, 1.000000000000000000 ) ) ;
#2196 = EDGE_CURVE ( 'NONE', #7049, #1427, #413, .T. ) ;
#2197 = VECTOR ( 'NONE', #4070, 1000.000000000000000 ) ;
#2198 = DIRECTION ( 'NONE',  ( 1.000000000000000000, 0.000000000000000000, 0.000000000000000000 ) ) ;
#2199 = EDGE_LOOP ( 'NONE', ( #7443, #8010, #5457 ) ) ;
#2200 = DIRECTION ( 'NONE',  ( -1.000000000000000000, -0.000000000000000000, -0.000000000000000000 ) ) ;
#2201 = ORIENTED_EDGE ( 'NONE', *, *, #135, .F. ) ;
#2202 = DIRECTION ( 'NONE',  ( -0.000000000000000000, -1.000000000000000000, -0.000000000000000000 ) ) ;
#2203 = DIRECTION ( 'NONE',  ( 0.000000000000000000, -1.000000000000000000, -1.460819769243626884E-16 ) ) ;
#2204 = LINE ( 'NONE', #1675, #50 ) ;
#2205 = LINE ( 'NONE', #5561, #421 ) ;
#2206 = EDGE_LOOP ( 'NONE', ( #2331, #1250, #6833, #157 ) ) ;
#2207 = VECTOR ( 'NONE', #5535, 1000.000000000000000 ) ;
#2208 = UNCERTAINTY_MEASURE_WITH_UNIT (LENGTH_MEASURE( 1.000000000000000082E-05 ), #5967, 'distance_accuracy_value', 'NONE');
#2209 = ORIENTED_EDGE ( 'NONE', *, *, #4753, .T. ) ;
#2210 = DIRECTION ( 'NONE',  ( -1.000000000000000000, 0.000000000000000000, 0.000000000000000000 ) ) ;
#2211 = EDGE_LOOP ( 'NONE', ( #6715, #5144 ) ) ;
#2212 = CYLINDRICAL_SURFACE ( 'NONE', #3779, 5.999999999999991118 ) ;
#2213 = DIRECTION ( 'NONE',  ( -0.000000000000000000, -7.945337353457666666E-18, -1.000000000000000000 ) ) ;
#2214 = VERTEX_POINT ( 'NONE', #1825 ) ;
#2215 = FACE_OUTER_BOUND ( 'NONE', #4169, .T. ) ;
#2216 = CIRCLE ( 'NONE', #5703, 8.999999999999994671 ) ;
#2217 = CARTESIAN_POINT ( 'NONE',  ( -105.9999999999999858, 114.9999999999999858, 10.00000000000000000 ) ) ;
#2218 = AXIS2_PLACEMENT_3D ( 'NONE', #1164, #611, #3096 ) ;
#2219 =( REPRESENTATION_RELATIONSHIP ('NONE','NONE', #6882, #3965 ) REPRESENTATION_RELATIONSHIP_WITH_TRANSFORMATION ( #1863 )SHAPE_REPRESENTATION_RELATIONSHIP( ) );
#2220 = FACE_OUTER_BOUND ( 'NONE', #1081, .T. ) ;
#2221 = LINE ( 'NONE', #4002, #783 ) ;
#2222 = DIRECTION ( 'NONE',  ( 0.000000000000000000, 0.000000000000000000, -1.000000000000000000 ) ) ;
#2223 = FACE_BOUND ( 'NONE', #7249, .T. ) ;
#2224 = PRODUCT_DEFINITION ( 'UNKNOWN', '', #3672, #7341 ) ;
#2225 = CARTESIAN_POINT ( 'NONE',  ( -125.0000000000000000, 125.0000000000000000, 0.000000000000000000 ) ) ;
#2226 = EDGE_LOOP ( 'NONE', ( #2246, #7149, #4337, #6802 ) ) ;
#2227 = ADVANCED_BREP_SHAPE_REPRESENTATION ( '', ( #931, #1299 ), #5023 ) ;
#2228 = EDGE_CURVE ( 'NONE', #5826, #6862, #6209, .T. ) ;
#2229 = EDGE_CURVE ( 'NONE', #5699, #7276, #6330, .T. ) ;
#2230 = CLOSED_SHELL ( 'NONE', ( #7292, #3818, #3695, #7103, #892, #4170, #7703, #2485, #7938, #579, #5920, #3689, #2276, #4404, #6905, #7013, #3012, #1757, #8269, #874, #137, #7115, #5151, #2721, #6602, #124, #3198, #4584, #3574, #8030, #1922, #2630, #6400, #4513, #2249, #7480, #6634, #7438, #4322, #3235, #7023, #2366, #4996, #982, #4732, #3586, #2579, #6350, #4357, #454, #5774, #3175, #5137, #87, #5192, #7718, #2171, #2926, #7211 ) ) ;
#2231 = EDGE_LOOP ( 'NONE', ( #6208, #6016, #4285, #1175 ) ) ;
#2232 = PLANE ( 'NONE',  #2406 ) ;
#2233 = DIRECTION ( 'NONE',  ( 1.000000000000000000, 0.000000000000000000, 0.000000000000000000 ) ) ;
#2234 = CONICAL_SURFACE ( 'NONE', #7068, 4.999999999999990230, 1.029744258676656754 ) ;
#2235 = ORIENTED_EDGE ( 'NONE', *, *, #1867, .T. ) ;
#2236 = CARTESIAN_POINT ( 'NONE',  ( -12.41819479434713891, -48.43362276422628554, -14.14586790793774895 ) ) ;
#2237 = SHAPE_REPRESENTATION_RELATIONSHIP ( 'NONE' , 'NONE' ,  #573, #6521 ) ;
#2238 = EDGE_CURVE ( 'NONE', #698, #1826, #5980, .T. ) ;
#2239 = CARTESIAN_POINT ( 'NONE',  ( 0.000000000000000000, 49.99999999999999289, -250.0000000000000000 ) ) ;
#2240 = CARTESIAN_POINT ( 'NONE',  ( -114.9999999999999147, -115.0000000000000000, 0.000000000000000000 ) ) ;
#2241 = VERTEX_POINT ( 'NONE', #716 ) ;
#2242 = CARTESIAN_POINT ( 'NONE',  ( 110.0000000000000142, -115.0000000000000000, 340.0000000000000000 ) ) ;
#2243 = CARTESIAN_POINT ( 'NONE',  ( 0.000000000000000000, 0.000000000000000000, 35.00000000000000000 ) ) ;
#2244 = ORIENTED_EDGE ( 'NONE', *, *, #7704, .F. ) ;
#2245 = DIRECTION ( 'NONE',  ( 1.000000000000000000, 0.000000000000000000, 0.000000000000000000 ) ) ;
#2246 = ORIENTED_EDGE ( 'NONE', *, *, #6540, .F. ) ;
#2247 = CARTESIAN_POINT ( 'NONE',  ( 115.0000000000000000, -114.9999999999999716, 10.00000000000000000 ) ) ;
#2248 = FACE_OUTER_BOUND ( 'NONE', #5783, .T. ) ;
#2249 = ADVANCED_FACE ( 'NONE', ( #7931 ), #5823, .T. ) ;
#2250 = CARTESIAN_POINT ( 'NONE',  ( 0.000000000000000000, 1.191800603018649864E-15, -100.0000000000000000 ) ) ;
#2251 = CARTESIAN_POINT ( 'NONE',  ( 115.0000000000000000, -115.0000000000000000, 270.0000000000000000 ) ) ;
#2252 = VERTEX_POINT ( 'NONE', #4669 ) ;
#2253 = ORIENTED_EDGE ( 'NONE', *, *, #8247, .T. ) ;
#2254 = DIRECTION ( 'NONE',  ( -1.000000000000000000, 0.000000000000000000, 0.000000000000000000 ) ) ;
#2255 = EDGE_LOOP ( 'NONE', ( #6356, #1114, #407, #3447 ) ) ;
#2256 = DIRECTION ( 'NONE',  ( 1.000000000000000000, -0.000000000000000000, 0.000000000000000000 ) ) ;
#2257 = PRODUCT_CONTEXT ( 'NONE', #6720, 'mechanical' ) ;
#2258 = ORIENTED_EDGE ( 'NONE', *, *, #2769, .F. ) ;
#2259 = CARTESIAN_POINT ( 'NONE',  ( 1.592040838891560279E-15, 105.0000000000000426, 92.99999999999992895 ) ) ;
#2260 = AXIS2_PLACEMENT_3D ( 'NONE', #3141, #1847, #7677 ) ;
#2261 = DIRECTION ( 'NONE',  ( -0.000000000000000000, -0.000000000000000000, 1.000000000000000000 ) ) ;
#2262 = CARTESIAN_POINT ( 'NONE',  ( -109.0000000000000426, -115.0000000000000000, 70.00000000000000000 ) ) ;
#2263 = DIRECTION ( 'NONE',  ( 0.000000000000000000, 0.4999999999999985012, -0.8660254037844393737 ) ) ;
#2264 = SHAPE_REPRESENTATION ( 'Bearing Housing', ( #1299 ), #2770 ) ;
#2265 = VERTEX_POINT ( 'NONE', #7253 ) ;
#2266 = AXIS2_PLACEMENT_3D ( 'NONE', #613, #1253, #7661 ) ;
#2267 = DIRECTION ( 'NONE',  ( 0.000000000000000000, 1.000000000000000000, 0.000000000000000000 ) ) ;
#2268 = EDGE_CURVE ( 'NONE', #1008, #7487, #3989, .T. ) ;
#2269 = CARTESIAN_POINT ( 'NONE',  ( -54.99999999999999289, -54.99999999999999289, 27.50000000000000000 ) ) ;
#2270 = EDGE_LOOP ( 'NONE', ( #5470, #1064 ) ) ;
#2271 = LINE ( 'NONE', #1121, #1308 ) ;
#2272 = VECTOR ( 'NONE', #2306, 1000.000000000000000 ) ;
#2273 = VECTOR ( 'NONE', #1587, 1000.000000000000000 ) ;
#2274 = DIRECTION ( 'NONE',  ( 1.000000000000000000, 0.000000000000000000, 0.000000000000000000 ) ) ;
#2275 = ORIENTED_EDGE ( 'NONE', *, *, #7081, .F. ) ;
#2276 = ADVANCED_FACE ( 'NONE', ( #2658 ), #2766, .F. ) ;
#2277 = VECTOR ( 'NONE', #6283, 1000.000000000000000 ) ;
#2278 = EDGE_CURVE ( 'NONE', #3595, #167, #7171, .T. ) ;
#2279 = EDGE_CURVE ( 'NONE', #8276, #5343, #7442, .T. ) ;
#2280 = DIRECTION ( 'NONE',  ( -0.000000000000000000, -0.000000000000000000, 1.000000000000000000 ) ) ;
#2281 = ORIENTED_EDGE ( 'NONE', *, *, #4563, .F. ) ;
#2282 = DIRECTION ( 'NONE',  ( 1.000000000000000000, 0.000000000000000000, 0.000000000000000000 ) ) ;
#2283 = FACE_OUTER_BOUND ( 'NONE', #2504, .T. ) ;
#2284 = CARTESIAN_POINT ( 'NONE',  ( 105.0000000000000000, 105.0000000000000568, 240.0000000000000284 ) ) ;
#2285 = CARTESIAN_POINT ( 'NONE',  ( 115.0000000000000000, -115.0000000000000000, 270.0000000000000000 ) ) ;
#2286 = CIRCLE ( 'NONE', #7538, 25.00000000000000000 ) ;
#2287 = VERTEX_POINT ( 'NONE', #1306 ) ;
#2288 = CARTESIAN_POINT ( 'NONE',  ( 120.5000000000000000, -114.9999999999999716, 10.00000000000000000 ) ) ;
#2289 = VECTOR ( 'NONE', #5780, 1000.000000000000000 ) ;
#2290 = VECTOR ( 'NONE', #3868, 1000.000000000000000 ) ;
#2291 = VERTEX_POINT ( 'NONE', #5276 ) ;
#2292 = CARTESIAN_POINT ( 'NONE',  ( -114.9999999999999147, 115.0000000000000000, 250.0000000000000000 ) ) ;
#2293 = DIRECTION ( 'NONE',  ( 0.000000000000000000, 0.000000000000000000, -1.000000000000000000 ) ) ;
#2294 = EDGE_LOOP ( 'NONE', ( #4985, #8133 ) ) ;
#2295 = DIRECTION ( 'NONE',  ( 1.460819769243626145E-16, -1.000000000000000000, 0.000000000000000000 ) ) ;
#2296 = AXIS2_PLACEMENT_3D ( 'NONE', #6352, #1256, #5080 ) ;
#2297 = AXIS2_PLACEMENT_3D ( 'NONE', #1037, #7497, #6690 ) ;
#2298 = EDGE_CURVE ( 'NONE', #179, #2535, #3370, .T. ) ;
#2299 = LINE ( 'NONE', #1061, #98 ) ;
#2300 = CARTESIAN_POINT ( 'NONE',  ( 8.909539772616881237E-14, 12.49999999999999822, 54.99999999999995026 ) ) ;
#2301 = VECTOR ( 'NONE', #7577, 1000.000000000000000 ) ;
#2302 = AXIS2_PLACEMENT_3D ( 'NONE', #6884, #6796, #6154 ) ;
#2303 = ORIENTED_EDGE ( 'NONE', *, *, #5622, .T. ) ;
#2304 = VECTOR ( 'NONE', #7793, 1000.000000000000000 ) ;
#2305 = ORIENTED_EDGE ( 'NONE', *, *, #3755, .F. ) ;
#2306 = DIRECTION ( 'NONE',  ( -1.000000000000000000, -0.000000000000000000, -0.000000000000000000 ) ) ;
#2307 = DIRECTION ( 'NONE',  ( 0.000000000000000000, 0.000000000000000000, -1.000000000000000000 ) ) ;
#2308 = DIRECTION ( 'NONE',  ( -0.000000000000000000, -0.000000000000000000, 1.000000000000000000 ) ) ;
#2309 = EDGE_LOOP ( 'NONE', ( #6537, #7695 ) ) ;
#2310 = CARTESIAN_POINT ( 'NONE',  ( -12.07658505203027843, -48.51980254810341364, -9.248211290718611366 ) ) ;
#2311 =( LENGTH_UNIT ( ) NAMED_UNIT ( * ) SI_UNIT ( .MILLI., .METRE. ) );
#2312 = ORIENTED_EDGE ( 'NONE', *, *, #5305, .T. ) ;
#2313 = DIRECTION ( 'NONE',  ( 1.000000000000000000, 0.000000000000000000, -0.000000000000000000 ) ) ;
#2314 = CARTESIAN_POINT ( 'NONE',  ( 114.9999999999999147, -115.0000000000000000, -28.00000000000002487 ) ) ;
#2315 = CYLINDRICAL_SURFACE ( 'NONE', #1073, 5.999999999999991118 ) ;
#2316 = ORIENTED_EDGE ( 'NONE', *, *, #7896, .T. ) ;
#2317 = FACE_OUTER_BOUND ( 'NONE', #4232, .T. ) ;
#2318 = DIRECTION ( 'NONE',  ( 1.000000000000000000, 0.000000000000000000, 0.000000000000000000 ) ) ;
#2319 = EDGE_LOOP ( 'NONE', ( #6583, #1120, #8295, #4661 ) ) ;
#2320 = CARTESIAN_POINT ( 'NONE',  ( -114.9999999999999716, 114.9999999999999858, 20.00000000000000000 ) ) ;
#2321 = LINE ( 'NONE', #2931, #7030 ) ;
#2322 = EDGE_CURVE ( 'NONE', #3289, #4789, #5282, .T. ) ;
#2323 = EDGE_CURVE ( 'NONE', #6249, #2457, #3389, .T. ) ;
#2324 = CIRCLE ( 'NONE', #140, 5.499999999999991118 ) ;
#2325 = CARTESIAN_POINT ( 'NONE',  ( 0.000000000000000000, 0.000000000000000000, 0.000000000000000000 ) ) ;
#2326 = EDGE_LOOP ( 'NONE', ( #4674, #6501, #5921, #1911 ) ) ;
#2327 = DIRECTION ( 'NONE',  ( 0.000000000000000000, -0.5000000000000011102, -0.8660254037844379305 ) ) ;
#2328 = PLANE ( 'NONE',  #7482 ) ;
#2329 = ORIENTED_EDGE ( 'NONE', *, *, #7065, .F. ) ;
#2330 = DIRECTION ( 'NONE',  ( 0.000000000000000000, 2.960594732333750610E-16, -1.000000000000000000 ) ) ;
#2331 = ORIENTED_EDGE ( 'NONE', *, *, #2487, .T. ) ;
#2332 = CONTEXT_DEPENDENT_SHAPE_REPRESENTATION ( #4622, #1370 ) ;
#2333 = ORIENTED_EDGE ( 'NONE', *, *, #1966, .T. ) ;
#2334 = DIRECTION ( 'NONE',  ( 0.000000000000000000, 0.000000000000000000, -1.000000000000000000 ) ) ;
#2335 = EDGE_CURVE ( 'NONE', #3678, #2601, #3117, .T. ) ;
#2336 = ORIENTED_EDGE ( 'NONE', *, *, #6917, .F. ) ;
#2337 = AXIS2_PLACEMENT_3D ( 'NONE', #3997, #5908, #4801 ) ;
#2338 = PLANE ( 'NONE',  #7252 ) ;
#2339 = ORIENTED_EDGE ( 'NONE', *, *, #7540, .T. ) ;
#2340 = DIRECTION ( 'NONE',  ( -0.000000000000000000, -0.000000000000000000, 1.000000000000000000 ) ) ;
#2341 = AXIS2_PLACEMENT_3D ( 'NONE', #1763, #7458, #3682 ) ;
#2342 = ORIENTED_EDGE ( 'NONE', *, *, #7806, .T. ) ;
#2343 = PRODUCT_DEFINITION_FORMATION_WITH_SPECIFIED_SOURCE ( 'ANY', '', #6606, .NOT_KNOWN. ) ;
#2344 = ORIENTED_EDGE ( 'NONE', *, *, #7429, .F. ) ;
#2345 = EDGE_CURVE ( 'NONE', #2252, #7231, #4050, .T. ) ;
#2346 = EDGE_LOOP ( 'NONE', ( #8111, #6761 ) ) ;
#2347 = CARTESIAN_POINT ( 'NONE',  ( 125.0000000000000000, 0.000000000000000000, 0.000000000000000000 ) ) ;
#2348 = EDGE_CURVE ( 'NONE', #6145, #8000, #1996, .T. ) ;
#2349 = LINE ( 'NONE', #6211, #112 ) ;
#2350 = CARTESIAN_POINT ( 'NONE',  ( -2.846087801003401196, -49.92054308009031161, -0.3214687869884009230 ) ) ;
#2351 =( LENGTH_UNIT ( ) NAMED_UNIT ( * ) SI_UNIT ( .MILLI., .METRE. ) );
#2352 = CLOSED_SHELL ( 'NONE', ( #2529, #8144, #3128, #5215, #2963, #5368, #2826, #3278, #4237, #5306, #134, #4458, #1362, #3668, #283, #8202, #4201, #1700, #8082, #2696, #5638, #258, #33, #7694, #6228, #5403, #8167, #4433, #3480, #5686, #725, #4774, #2725 ) ) ;
#2353 = ORIENTED_EDGE ( 'NONE', *, *, #7980, .T. ) ;
#2354 = DIRECTION ( 'NONE',  ( 0.000000000000000000, 0.000000000000000000, -1.000000000000000000 ) ) ;
#2355 = AXIS2_PLACEMENT_3D ( 'NONE', #5502, #5073, #565 ) ;
#2356 = FACE_OUTER_BOUND ( 'NONE', #2851, .T. ) ;
#2357 = PLANE ( 'NONE',  #2368 ) ;
#2358 = ORIENTED_EDGE ( 'NONE', *, *, #4152, .T. ) ;
#2359 = DIRECTION ( 'NONE',  ( -0.000000000000000000, -0.000000000000000000, 1.000000000000000000 ) ) ;
#2360 = DIRECTION ( 'NONE',  ( -0.000000000000000000, -0.000000000000000000, 1.000000000000000000 ) ) ;
#2361 = EDGE_LOOP ( 'NONE', ( #8298, #1263, #5982, #365 ) ) ;
#2362 = DIRECTION ( 'NONE',  ( 1.000000000000000000, 0.000000000000000000, 0.000000000000000000 ) ) ;
#2363 = ORIENTED_EDGE ( 'NONE', *, *, #5060, .T. ) ;
#2364 = LINE ( 'NONE', #1642, #2683 ) ;
#2365 = ORIENTED_EDGE ( 'NONE', *, *, #2427, .F. ) ;
#2366 = ADVANCED_FACE ( 'NONE', ( #801 ), #8108, .F. ) ;
#2367 = CARTESIAN_POINT ( 'NONE',  ( -115.0000000000000284, -115.0000000000000000, 70.00000000000000000 ) ) ;
#2368 = AXIS2_PLACEMENT_3D ( 'NONE', #2922, #1670, #8264 ) ;
#2369 = CARTESIAN_POINT ( 'NONE',  ( 125.0000000000000000, 120.0000000000000000, 0.000000000000000000 ) ) ;
#2370 = APPLICATION_CONTEXT ( 'automotive_design' ) ;
#2371 = ITEM_DEFINED_TRANSFORMATION ( 'NONE', 'NONE', #5837,  #1299 ) ;
#2372 = VERTEX_POINT ( 'NONE', #5312 ) ;
#2373 = LINE ( 'NONE', #3563, #1913 ) ;
#2374 = ORIENTED_EDGE ( 'NONE', *, *, #2964, .T. ) ;
#2375 = LINE ( 'NONE', #6789, #2207 ) ;
#2376 = EDGE_LOOP ( 'NONE', ( #6968, #5734 ) ) ;
#2377 = LINE ( 'NONE', #5538, #4951 ) ;
#2378 = ORIENTED_EDGE ( 'NONE', *, *, #2977, .F. ) ;
#2379 = EDGE_CURVE ( 'NONE', #1680, #7933, #1474, .T. ) ;
#2380 = CYLINDRICAL_SURFACE ( 'NONE', #2302, 5.499999999999991118 ) ;
#2381 = ADVANCED_FACE ( 'NONE', ( #5859 ), #25, .T. ) ;
#2382 = EDGE_CURVE ( 'NONE', #402, #5627, #4177, .T. ) ;
#2383 = DIRECTION ( 'NONE',  ( 1.000000000000000000, 0.000000000000000000, 0.000000000000000000 ) ) ;
#2384 = ORIENTED_EDGE ( 'NONE', *, *, #4773, .F. ) ;
#2385 =( NAMED_UNIT ( * ) SI_UNIT ( $, .STERADIAN. ) SOLID_ANGLE_UNIT ( ) );
#2386 = EDGE_LOOP ( 'NONE', ( #59, #3390 ) ) ;
#2387 = DIRECTION ( 'NONE',  ( 0.000000000000000000, 1.000000000000000000, 0.000000000000000000 ) ) ;
#2388 = EDGE_CURVE ( 'NONE', #7988, #7828, #2205, .T. ) ;
#2389 = VECTOR ( 'NONE', #2521, 1000.000000000000000 ) ;
#2390 = CARTESIAN_POINT ( 'NONE',  ( -121.0000000000000284, -115.0000000000000000, 70.00000000000000000 ) ) ;
#2391 = CARTESIAN_POINT ( 'NONE',  ( -8.554558110533214688, -49.26362287191481215, -3.376715202643650215 ) ) ;
#2392 = AXIS2_PLACEMENT_3D ( 'NONE', #1242, #7097, #6374 ) ;
#2393 = AXIS2_PLACEMENT_3D ( 'NONE', #3814, #2436, #6465 ) ;
#2394 = ORIENTED_EDGE ( 'NONE', *, *, #4348, .F. ) ;
#2395 = CARTESIAN_POINT ( 'NONE',  ( -54.99999999999999289, -55.00000000000000711, 27.50000000000000000 ) ) ;
#2396 = FACE_BOUND ( 'NONE', #1193, .T. ) ;
#2397 = DIRECTION ( 'NONE',  ( -0.000000000000000000, -0.000000000000000000, 1.000000000000000000 ) ) ;
#2398 = ADVANCED_FACE ( 'NONE', ( #5522, #3511 ), #8130, .T. ) ;
#2399 = AXIS2_PLACEMENT_3D ( 'NONE', #6177, #998, #3636 ) ;
#2400 = EDGE_LOOP ( 'NONE', ( #4395, #3990 ) ) ;
#2401 = DIRECTION ( 'NONE',  ( 0.000000000000000000, -1.000000000000000000, 1.266875999117951024E-16 ) ) ;
#2402 = DIRECTION ( 'NONE',  ( -0.000000000000000000, -0.000000000000000000, 1.000000000000000000 ) ) ;
#2403 = EDGE_LOOP ( 'NONE', ( #7213, #1856, #1606, #4809, #4115, #6782, #5578, #1788 ) ) ;
#2404 = SURFACE_STYLE_FILL_AREA ( #3646 ) ;
#2405 = CARTESIAN_POINT ( 'NONE',  ( 1.000000000000000888, 9.797174393178827630E-16, 8.000000000000000000 ) ) ;
#2406 = AXIS2_PLACEMENT_3D ( 'NONE', #6077, #130, #6040 ) ;
#2407 = AXIS2_PLACEMENT_3D ( 'NONE', #3647, #6226, #1219 ) ;
#2408 = EDGE_LOOP ( 'NONE', ( #438, #7740 ) ) ;
#2409 = LINE ( 'NONE', #5050, #7543 ) ;
#2410 = DIRECTION ( 'NONE',  ( -0.000000000000000000, -0.000000000000000000, -1.000000000000000000 ) ) ;
#2411 = ORIENTED_EDGE ( 'NONE', *, *, #2860, .F. ) ;
#2412 = FACE_OUTER_BOUND ( 'NONE', #6937, .T. ) ;
#2413 = CARTESIAN_POINT ( 'NONE',  ( 17.61817604250836311, 4.500000000000000000, -28.00000000000002487 ) ) ;
#2414 = AXIS2_PLACEMENT_3D ( 'NONE', #3771, #1320, #7059 ) ;
#2415 = APPLICATION_PROTOCOL_DEFINITION ( 'draft international standard', 'automotive_design', 1998, #5860 ) ;
#2416 = VECTOR ( 'NONE', #4711, 1000.000000000000000 ) ;
#2417 = ORIENTED_EDGE ( 'NONE', *, *, #7552, .T. ) ;
#2418 = CARTESIAN_POINT ( 'NONE',  ( 5.169052467613985513, 49.73353547763981908, -23.88849205255369412 ) ) ;
#2419 = ORIENTED_EDGE ( 'NONE', *, *, #3638, .T. ) ;
#2420 = FACE_OUTER_BOUND ( 'NONE', #480, .T. ) ;
#2421 = DIRECTION ( 'NONE',  ( 0.000000000000000000, 0.000000000000000000, 1.000000000000000000 ) ) ;
#2422 = CARTESIAN_POINT ( 'NONE',  ( 0.000000000000000000, 4.500000000000000000, -128.0000120000000265 ) ) ;
#2423 = AXIS2_PLACEMENT_3D ( 'NONE', #5830, #5321, #1442 ) ;
#2424 = FACE_OUTER_BOUND ( 'NONE', #1485, .T. ) ;
#2425 = DIRECTION ( 'NONE',  ( 0.000000000000000000, 1.000000000000000000, 0.000000000000000000 ) ) ;
#2426 = ORIENTED_EDGE ( 'NONE', *, *, #680, .T. ) ;
#2427 = EDGE_CURVE ( 'NONE', #1534, #3826, #1512, .T. ) ;
#2428 = ORIENTED_EDGE ( 'NONE', *, *, #1484, .T. ) ;
#2429 = EDGE_CURVE ( 'NONE', #501, #929, #2324, .T. ) ;
#2430 = EDGE_CURVE ( 'NONE', #509, #6613, #6898, .T. ) ;
#2431 = CARTESIAN_POINT ( 'NONE',  ( -75.00000000000000000, 75.00000000000000000, 27.50000000000000000 ) ) ;
#2432 = AXIS2_PLACEMENT_3D ( 'NONE', #1469, #102, #7333 ) ;
#2433 = CIRCLE ( 'NONE', #4974, 25.00000000000000000 ) ;
#2434 = CARTESIAN_POINT ( 'NONE',  ( 0.000000000000000000, 125.0000000000000568, 66.99999999999992895 ) ) ;
#2435 = ORIENTED_EDGE ( 'NONE', *, *, #8135, .T. ) ;
#2436 = DIRECTION ( 'NONE',  ( -0.000000000000000000, -0.000000000000000000, 1.000000000000000000 ) ) ;
#2437 = CARTESIAN_POINT ( 'NONE',  ( 7.910144901597300363E-14, 88.75000000000001421, -282.0000000000000568 ) ) ;
#2438 = AXIS2_PLACEMENT_3D ( 'NONE', #7024, #1206, #605 ) ;
#2439 = ORIENTED_EDGE ( 'NONE', *, *, #7821, .T. ) ;
#2440 = AXIS2_PLACEMENT_3D ( 'NONE', #8286, #304, #1920 ) ;
#2441 = ADVANCED_FACE ( 'NONE', ( #1045 ), #7338, .F. ) ;
#2442 = CARTESIAN_POINT ( 'NONE',  ( 10.40000000000000036, 6.613092715395750854E-16, 5.400000000000035882 ) ) ;
#2443 = CARTESIAN_POINT ( 'NONE',  ( -94.99999999999997158, -95.00000000000008527, 35.00000000000000000 ) ) ;
#2444 = CARTESIAN_POINT ( 'NONE',  ( 20.76917701662883076, 0.000000000000000000, 0.000000000000000000 ) ) ;
#2445 = ORIENTED_EDGE ( 'NONE', *, *, #5036, .T. ) ;
#2446 = DIRECTION ( 'NONE',  ( 0.000000000000000000, -0.000000000000000000, -1.000000000000000000 ) ) ;
#2447 = CARTESIAN_POINT ( 'NONE',  ( 109.0000000000000142, 115.0000000000000000, 70.00000000000000000 ) ) ;
#2448 = ORIENTED_EDGE ( 'NONE', *, *, #3237, .F. ) ;
#2449 = FILL_AREA_STYLE_COLOUR ( '', #2879 ) ;
#2450 = PRODUCT_DEFINITION_SHAPE ( 'NONE', 'NONE',  #8350 ) ;
#2451 = CARTESIAN_POINT ( 'NONE',  ( 95.00000000000002842, -95.00000000000002842, 70.00000000000000000 ) ) ;
#2452 = EDGE_CURVE ( 'NONE', #4851, #2735, #700, .T. ) ;
#2453 = DIRECTION ( 'NONE',  ( 0.000000000000000000, -0.4999999999999985012, 0.8660254037844393737 ) ) ;
#2454 = UNCERTAINTY_MEASURE_WITH_UNIT (LENGTH_MEASURE( 1.000000000000000082E-05 ), #5550, 'distance_accuracy_value', 'NONE');
#2455 = ORIENTED_EDGE ( 'NONE', *, *, #5475, .T. ) ;
#2456 = DIRECTION ( 'NONE',  ( -0.7071067811865420216, 0.000000000000000000, 0.7071067811865531239 ) ) ;
#2457 = VERTEX_POINT ( 'NONE', #355 ) ;
#2458 = CARTESIAN_POINT ( 'NONE',  ( -59.99999999999999289, -55.00000000000000000, 220.0000000000000284 ) ) ;
#2459 = DIRECTION ( 'NONE',  ( -0.000000000000000000, -0.000000000000000000, 1.000000000000000000 ) ) ;
#2460 = APPLICATION_PROTOCOL_DEFINITION ( 'draft international standard', 'automotive_design', 1998, #8297 ) ;
#2461 = ORIENTED_EDGE ( 'NONE', *, *, #7161, .F. ) ;
#2462 = CARTESIAN_POINT ( 'NONE',  ( 12.07658505203027843, 48.51980254810342075, -9.248211290718606037 ) ) ;
#2463 = ORIENTED_EDGE ( 'NONE', *, *, #1980, .T. ) ;
#2464 = DIRECTION ( 'NONE',  ( -1.000000000000000000, 0.000000000000000000, 0.000000000000000000 ) ) ;
#2465 = ORIENTED_EDGE ( 'NONE', *, *, #3174, .F. ) ;
#2466 = CARTESIAN_POINT ( 'NONE',  ( -49.00000000000000000, -55.00000000000000711, 27.50000000000000000 ) ) ;
#2467 = CARTESIAN_POINT ( 'NONE',  ( 17.61817604250836311, -4.500000000000000000, -118.0000000000000284 ) ) ;
#2468 = EDGE_LOOP ( 'NONE', ( #1239, #4779, #1155, #3877, #4051, #5086, #6552, #1588 ) ) ;
#2469 = EDGE_LOOP ( 'NONE', ( #2258, #6415 ) ) ;
#2470 = DIRECTION ( 'NONE',  ( -0.000000000000000000, -7.945337353457666666E-18, -1.000000000000000000 ) ) ;
#2471 = EDGE_CURVE ( 'NONE', #1962, #4206, #4109, .T. ) ;
#2472 = CONICAL_SURFACE ( 'NONE', #3513, 5.999999999999991118, 1.029744258676652313 ) ;
#2473 = CARTESIAN_POINT ( 'NONE',  ( 114.9999999999999147, 115.0000000000000000, -28.00000000000002487 ) ) ;
#2474 = EDGE_CURVE ( 'NONE', #2571, #7082, #3245, .T. ) ;
#2475 = ORIENTED_EDGE ( 'NONE', *, *, #3825, .F. ) ;
#2476 = DIRECTION ( 'NONE',  ( 0.000000000000000000, 1.460819769243626884E-16, 1.000000000000000000 ) ) ;
#2477 = CARTESIAN_POINT ( 'NONE',  ( -1.551748806516483090E-14, -88.75000000000000000, -94.50000000000011369 ) ) ;
#2478 = CIRCLE ( 'NONE', #2341, 5.999999999999991118 ) ;
#2479 = PRODUCT_DEFINITION_FORMATION_WITH_SPECIFIED_SOURCE ( 'ANY', '', #7427, .NOT_KNOWN. ) ;
#2480 = CARTESIAN_POINT ( 'NONE',  ( -75.00000000000000000, 0.000000000000000000, 12.50000000000000000 ) ) ;
#2481 = APPLICATION_CONTEXT ( 'automotive_design' ) ;
#2482 = FACE_BOUND ( 'NONE', #3016, .T. ) ;
#2483 = DIRECTION ( 'NONE',  ( -1.000000000000000000, 0.000000000000000000, 0.000000000000000000 ) ) ;
#2484 = EDGE_CURVE ( 'NONE', #5937, #3656, #1639, .T. ) ;
#2485 = ADVANCED_FACE ( 'NONE', ( #6057 ), #4862, .F. ) ;
#2486 = CARTESIAN_POINT ( 'NONE',  ( 9.123515037571451103, -49.16144051280858207, -21.05438506594878234 ) ) ;
#2487 = EDGE_CURVE ( 'NONE', #6953, #3210, #2321, .T. ) ;
#2488 = DIRECTION ( 'NONE',  ( -0.000000000000000000, -0.000000000000000000, 1.000000000000000000 ) ) ;
#2489 = CARTESIAN_POINT ( 'NONE',  ( 109.0000000000000426, -115.0000000000000000, 20.00000000000000355 ) ) ;
#2490 = ORIENTED_EDGE ( 'NONE', *, *, #6181, .F. ) ;
#2491 = ORIENTED_EDGE ( 'NONE', *, *, #7743, .F. ) ;
#2492 = EDGE_LOOP ( 'NONE', ( #7433, #292 ) ) ;
#2493 = CARTESIAN_POINT ( 'NONE',  ( 60.00000000000000000, -55.00000000000000000, 240.0000000000000284 ) ) ;
#2494 = CARTESIAN_POINT ( 'NONE',  ( 0.000000000000000000, 0.000000000000000000, 70.00000000000000000 ) ) ;
#2495 = EDGE_LOOP ( 'NONE', ( #4227, #7457, #7004, #2728 ) ) ;
#2496 = CARTESIAN_POINT ( 'NONE',  ( -105.0000000000000000, 105.0000000000000853, 20.00000000000000355 ) ) ;
#2497 = DIRECTION ( 'NONE',  ( -0.000000000000000000, -0.000000000000000000, 1.000000000000000000 ) ) ;
#2498 = ORIENTED_EDGE ( 'NONE', *, *, #6788, .T. ) ;
#2499 = PRODUCT_CONTEXT ( 'NONE', #5106, 'mechanical' ) ;
#2500 = VERTEX_POINT ( 'NONE', #7466 ) ;
#2501 = CARTESIAN_POINT ( 'NONE',  ( 12.41960978562214102, 48.43326235599739960, -10.86247626165360813 ) ) ;
#2502 = ORIENTED_EDGE ( 'NONE', *, *, #4796, .T. ) ;
#2503 = CARTESIAN_POINT ( 'NONE',  ( 0.000000000000000000, 125.0000000000000568, 66.99999999999992895 ) ) ;
#2504 = EDGE_LOOP ( 'NONE', ( #2693, #207, #1057, #4728 ) ) ;
#2505 =( LENGTH_UNIT ( ) NAMED_UNIT ( * ) SI_UNIT ( .MILLI., .METRE. ) );
#2506 = CARTESIAN_POINT ( 'NONE',  ( -11.83910760917652460, 48.57829327830486221, -16.53147691254502760 ) ) ;
#2507 = ORIENTED_EDGE ( 'NONE', *, *, #5064, .T. ) ;
#2508 = DIRECTION ( 'NONE',  ( -0.000000000000000000, -0.000000000000000000, -1.000000000000000000 ) ) ;
#2509 = CARTESIAN_POINT ( 'NONE',  ( -75.00000000000001421, 0.000000000000000000, 20.00000000000000000 ) ) ;
#2510 = ORIENTED_EDGE ( 'NONE', *, *, #3825, .T. ) ;
#2511 = DIRECTION ( 'NONE',  ( 1.000000000000000000, 0.000000000000000000, 0.000000000000000000 ) ) ;
#2512 = CARTESIAN_POINT ( 'NONE',  ( -1.110223024625156540E-13, -12.50000000000001066, 1.387778780781445676E-14 ) ) ;
#2513 = PRODUCT_DEFINITION_SHAPE ( 'NONE', 'NONE',  #8354 ) ;
#2514 = DIRECTION ( 'NONE',  ( -0.000000000000000000, -0.000000000000000000, 1.000000000000000000 ) ) ;
#2515 = ORIENTED_EDGE ( 'NONE', *, *, #4888, .T. ) ;
#2516 = VECTOR ( 'NONE', #6500, 1000.000000000000000 ) ;
#2517 = EDGE_CURVE ( 'NONE', #4954, #6358, #2712, .T. ) ;
#2518 = CARTESIAN_POINT ( 'NONE',  ( -115.0000000000000000, -115.0000000000000000, 270.0000000000000000 ) ) ;
#2519 = AXIS2_PLACEMENT_3D ( 'NONE', #6683, #3377, #2838 ) ;
#2520 = PLANE ( 'NONE',  #5108 ) ;
#2521 = DIRECTION ( 'NONE',  ( 0.000000000000000000, -1.000000000000000000, 9.256405414277014607E-16 ) ) ;
#2522 = CARTESIAN_POINT ( 'NONE',  ( -114.9999999999999858, -114.9999999999999858, 20.00000000000000000 ) ) ;
#2523 =( GEOMETRIC_REPRESENTATION_CONTEXT ( 3 ) GLOBAL_UNCERTAINTY_ASSIGNED_CONTEXT ( ( #8097 ) ) GLOBAL_UNIT_ASSIGNED_CONTEXT ( ( #425, #7400, #2385 ) ) REPRESENTATION_CONTEXT ( 'NONE', 'WORKASPACE' ) );
#2524 = DIRECTION ( 'NONE',  ( -0.000000000000000000, -0.000000000000000000, 1.000000000000000000 ) ) ;
#2525 = ORIENTED_EDGE ( 'NONE', *, *, #3782, .F. ) ;
#2526 = CARTESIAN_POINT ( 'NONE',  ( -102.5000000000000000, 0.000000000000000000, -9.500000000000008882 ) ) ;
#2527 = EDGE_CURVE ( 'NONE', #6613, #509, #7248, .T. ) ;
#2528 = EDGE_CURVE ( 'NONE', #4692, #3799, #2540, .T. ) ;
#2529 = ADVANCED_FACE ( 'NONE', ( #4225 ), #3601, .F. ) ;
#2530 = CONICAL_SURFACE ( 'NONE', #3578, 5.999999999999991118, 1.029744258676652313 ) ;
#2531 = ORIENTED_EDGE ( 'NONE', *, *, #3653, .F. ) ;
#2532 = PRODUCT_DEFINITION_CONTEXT ( 'detailed design', #3212, 'design' ) ;
#2533 = ORIENTED_EDGE ( 'NONE', *, *, #4785, .F. ) ;
#2534 = LINE ( 'NONE', #2493, #2290 ) ;
#2535 = VERTEX_POINT ( 'NONE', #7971 ) ;
#2536 = DIRECTION ( 'NONE',  ( -0.8571673007021134438, 1.049727191138620051E-16, 0.5150380749100522682 ) ) ;
#2537 = DIRECTION ( 'NONE',  ( 1.000000000000000000, 0.000000000000000000, 0.000000000000000000 ) ) ;
#2538 = CIRCLE ( 'NONE', #7244, 5.999999999999991118 ) ;
#2539 = DIRECTION ( 'NONE',  ( 0.8571673007021134438, 0.000000000000000000, 0.5150380749100522682 ) ) ;
#2540 = CIRCLE ( 'NONE', #7118, 9.000000000000007105 ) ;
#2541 = DIRECTION ( 'NONE',  ( 1.000000000000000000, 0.000000000000000000, 0.000000000000000000 ) ) ;
#2542 = VECTOR ( 'NONE', #5245, 1000.000000000000000 ) ;
#2543 = FACE_OUTER_BOUND ( 'NONE', #4119, .T. ) ;
#2544 = VECTOR ( 'NONE', #6864, 1000.000000000000000 ) ;
#2545 = AXIS2_PLACEMENT_3D ( 'NONE', #844, #759, #5351 ) ;
#2546 = FACE_OUTER_BOUND ( 'NONE', #6856, .T. ) ;
#2547 = ORIENTED_EDGE ( 'NONE', *, *, #5060, .F. ) ;
#2548 = ADVANCED_FACE ( 'NONE', ( #6186 ), #404, .F. ) ;
#2549 = CARTESIAN_POINT ( 'NONE',  ( 0.000000000000000000, 52.49999999999997868, 79.99999999999994316 ) ) ;
#2550 = CARTESIAN_POINT ( 'NONE',  ( 114.9999999999999147, 0.000000000000000000, 0.000000000000000000 ) ) ;
#2551 = DIRECTION ( 'NONE',  ( 1.000000000000000000, 0.000000000000000000, 0.000000000000000000 ) ) ;
#2552 = AXIS2_PLACEMENT_3D ( 'NONE', #7127, #4450, #7042 ) ;
#2553 = AXIS2_PLACEMENT_3D ( 'NONE', #709, #3266, #5935 ) ;
#2554 = DIRECTION ( 'NONE',  ( -1.000000000000000000, 0.000000000000000000, 0.000000000000000000 ) ) ;
#2555 = ORIENTED_EDGE ( 'NONE', *, *, #2912, .F. ) ;
#2556 = CARTESIAN_POINT ( 'NONE',  ( 1.387778780781445676E-14, 1.336063342249516596E-14, -94.50000000000000000 ) ) ;
#2557 = ORIENTED_EDGE ( 'NONE', *, *, #3827, .F. ) ;
#2558 = ORIENTED_EDGE ( 'NONE', *, *, #3873, .F. ) ;
#2559 = AXIS2_PLACEMENT_3D ( 'NONE', #1504, #2145, #3940 ) ;
#2560 = AXIS2_PLACEMENT_3D ( 'NONE', #6311, #5200, #7545 ) ;
#2561 = CARTESIAN_POINT ( 'NONE',  ( 14.30908802125418511, 4.500000000000000000, -28.00000000000002487 ) ) ;
#2562 = CARTESIAN_POINT ( 'NONE',  ( -125.0000000000000000, 125.0000000000000000, -28.00000000000002487 ) ) ;
#2563 = CARTESIAN_POINT ( 'NONE',  ( 9.920070434648168956, -49.00675803034337719, -20.11641848348691042 ) ) ;
#2564 = VECTOR ( 'NONE', #6472, 1000.000000000000000 ) ;
#2565 = CARTESIAN_POINT ( 'NONE',  ( 125.0000000000000000, 52.50000000000000000, 190.0000000000000284 ) ) ;
#2566 = DIRECTION ( 'NONE',  ( -0.000000000000000000, -1.000000000000000000, -0.000000000000000000 ) ) ;
#2567 = CARTESIAN_POINT ( 'NONE',  ( 120.0000000000000000, -125.0000000000000000, -28.00000000000002487 ) ) ;
#2568 = ORIENTED_EDGE ( 'NONE', *, *, #3133, .T. ) ;
#2569 = CARTESIAN_POINT ( 'NONE',  ( 10.00000000000000000, -3.448762466456902719E-14, 93.74999999999998579 ) ) ;
#2570 = VECTOR ( 'NONE', #6633, 1000.000000000000000 ) ;
#2571 = VERTEX_POINT ( 'NONE', #2489 ) ;
#2572 = VERTEX_POINT ( 'NONE', #6355 ) ;
#2573 = CARTESIAN_POINT ( 'NONE',  ( -25.00000000000000000, 0.000000000000000000, -128.0000000000000284 ) ) ;
#2574 = PRODUCT_RELATED_PRODUCT_CATEGORY ( 'part', '', ( #6606 ) ) ;
#2575 = VERTEX_POINT ( 'NONE', #1092 ) ;
#2576 = CARTESIAN_POINT ( 'NONE',  ( 5.000000000000000000, -4.685197434473809430, 7.372574772901430151E-15 ) ) ;
#2577 = DIRECTION ( 'NONE',  ( -0.000000000000000000, -0.000000000000000000, 1.000000000000000000 ) ) ;
#2578 = ADVANCED_FACE ( 'NONE', ( #4354 ), #1813, .T. ) ;
#2579 = ADVANCED_FACE ( 'NONE', ( #3787 ), #7036, .F. ) ;
#2580 = EDGE_LOOP ( 'NONE', ( #8196, #4007, #1468, #8242 ) ) ;
#2581 = CARTESIAN_POINT ( 'NONE',  ( 10.16275934324372621, 48.95683464664498530, -19.78926114801199532 ) ) ;
#2582 = ORIENTED_EDGE ( 'NONE', *, *, #1990, .F. ) ;
#2583 = CARTESIAN_POINT ( 'NONE',  ( -125.0000000000000000, -52.49999999999997158, 0.000000000000000000 ) ) ;
#2584 = CARTESIAN_POINT ( 'NONE',  ( -125.0000000000002558, -125.0000000000000000, 0.000000000000000000 ) ) ;
#2585 = EDGE_CURVE ( 'NONE', #6321, #2993, #4961, .T. ) ;
#2586 = ORIENTED_EDGE ( 'NONE', *, *, #510, .T. ) ;
#2587 = CARTESIAN_POINT ( 'NONE',  ( 115.0000000000000000, -115.0000000000000000, 270.0000000000000000 ) ) ;
#2588 = EDGE_CURVE ( 'NONE', #8205, #7327, #442, .T. ) ;
#2589 = EDGE_LOOP ( 'NONE', ( #7615, #4290, #6395, #5202 ) ) ;
#2590 = ADVANCED_FACE ( 'NONE', ( #538 ), #8179, .F. ) ;
#2591 = DIRECTION ( 'NONE',  ( -0.000000000000000000, -0.000000000000000000, -1.000000000000000000 ) ) ;
#2592 = ORIENTED_EDGE ( 'NONE', *, *, #2183, .T. ) ;
#2593 = AXIS2_PLACEMENT_3D ( 'NONE', #1517, #6742, #230 ) ;
#2594 = DIRECTION ( 'NONE',  ( -0.000000000000000000, -0.000000000000000000, 1.000000000000000000 ) ) ;
#2595 = LINE ( 'NONE', #1973, #6878 ) ;
#2596 = ORIENTED_EDGE ( 'NONE', *, *, #2379, .F. ) ;
#2597 = EDGE_CURVE ( 'NONE', #5626, #5018, #1133, .T. ) ;
#2598 = CARTESIAN_POINT ( 'NONE',  ( -0.8183949479883554368, -49.99498560413270809, -24.97998898815200874 ) ) ;
#2599 = CARTESIAN_POINT ( 'NONE',  ( -1.615572193008695713E-14, -88.75000000000000000, -282.0000000000000568 ) ) ;
#2600 = ORIENTED_EDGE ( 'NONE', *, *, #7000, .F. ) ;
#2601 = VERTEX_POINT ( 'NONE', #2405 ) ;
#2602 = CIRCLE ( 'NONE', #1118, 4.057500000000000107 ) ;
#2603 = CARTESIAN_POINT ( 'NONE',  ( 25.00000000000000000, 3.061616997868383043E-15, -128.0000000000000284 ) ) ;
#2604 = DIRECTION ( 'NONE',  ( 0.000000000000000000, 1.000000000000000000, -9.256405414277014607E-16 ) ) ;
#2605 = CARTESIAN_POINT ( 'NONE',  ( -1.110223024625156540E-13, -12.50000000000001066, 1.387778780781445676E-14 ) ) ;
#2606 = DIRECTION ( 'NONE',  ( 1.000000000000000000, 0.000000000000000000, 0.000000000000000000 ) ) ;
#2607 = AXIS2_PLACEMENT_3D ( 'NONE', #2512, #5752, #7022 ) ;
#2608 = DIRECTION ( 'NONE',  ( 0.000000000000000000, 2.960594732333750117E-16, -1.000000000000000000 ) ) ;
#2609 = AXIS2_PLACEMENT_3D ( 'NONE', #3291, #8054, #5295 ) ;
#2610 = DIRECTION ( 'NONE',  ( -0.000000000000000000, -1.000000000000000000, 1.586032892321652236E-16 ) ) ;
#2611 = ORIENTED_EDGE ( 'NONE', *, *, #6278, .T. ) ;
#2612 = VERTEX_POINT ( 'NONE', #3108 ) ;
#2613 = ORIENTED_EDGE ( 'NONE', *, *, #7528, .F. ) ;
#2614 = DIRECTION ( 'NONE',  ( -0.000000000000000000, -1.000000000000000000, 1.586032892321652236E-16 ) ) ;
#2615 = ORIENTED_EDGE ( 'NONE', *, *, #5679, .T. ) ;
#2616 = EDGE_CURVE ( 'NONE', #4104, #3739, #5336, .T. ) ;
#2617 = DIRECTION ( 'NONE',  ( -1.000000000000000000, -0.000000000000000000, -0.000000000000000000 ) ) ;
#2618 = FACE_OUTER_BOUND ( 'NONE', #625, .T. ) ;
#2619 = CARTESIAN_POINT ( 'NONE',  ( 5.000000000000000000, -4.685197434473809430, 7.372574772901430151E-15 ) ) ;
#2620 = VECTOR ( 'NONE', #1116, 1000.000000000000000 ) ;
#2621 = ADVANCED_FACE ( 'NONE', ( #578 ), #7594, .T. ) ;
#2622 = DIRECTION ( 'NONE',  ( -2.921639538487254261E-16, 1.000000000000000000, 0.000000000000000000 ) ) ;
#2623 = LINE ( 'NONE', #1872, #6579 ) ;
#2624 = ORIENTED_EDGE ( 'NONE', *, *, #4419, .T. ) ;
#2625 = LINE ( 'NONE', #4462, #1809 ) ;
#2626 = ORIENTED_EDGE ( 'NONE', *, *, #8258, .F. ) ;
#2627 = LINE ( 'NONE', #3996, #2932 ) ;
#2628 = MECHANICAL_DESIGN_GEOMETRIC_PRESENTATION_REPRESENTATION (  '', ( #2111 ), #464 ) ;
#2629 = ORIENTED_EDGE ( 'NONE', *, *, #2379, .T. ) ;
#2630 = ADVANCED_FACE ( 'NONE', ( #3143, #7551, #6266, #4265, #489, #4443 ), #3058, .F. ) ;
#2631 = CARTESIAN_POINT ( 'NONE',  ( -109.4999999999999858, 114.9999999999999858, 20.00000000000000000 ) ) ;
#2632 = EDGE_CURVE ( 'NONE', #7988, #3069, #1850, .T. ) ;
#2633 = DIRECTION ( 'NONE',  ( -0.000000000000000000, -0.000000000000000000, -1.000000000000000000 ) ) ;
#2634 = DIRECTION ( 'NONE',  ( -0.000000000000000000, -0.000000000000000000, 1.000000000000000000 ) ) ;
#2635 = DIRECTION ( 'NONE',  ( -0.000000000000000000, -0.000000000000000000, 1.000000000000000000 ) ) ;
#2636 = ORIENTED_EDGE ( 'NONE', *, *, #4631, .F. ) ;
#2637 = FACE_BOUND ( 'NONE', #7473, .T. ) ;
#2638 = SHAPE_DEFINITION_REPRESENTATION ( #2112, #6882 ) ;
#2639 = ORIENTED_EDGE ( 'NONE', *, *, #5260, .T. ) ;
#2640 = EDGE_CURVE ( 'NONE', #1680, #1522, #5005, .T. ) ;
#2641 = FACE_OUTER_BOUND ( 'NONE', #6826, .T. ) ;
#2642 = DIRECTION ( 'NONE',  ( -1.000000000000000000, -2.643388153869419325E-16, 0.000000000000000000 ) ) ;
#2643 = CARTESIAN_POINT ( 'NONE',  ( 8.258796090566862702, -49.31668406204209276, -21.91840799305901299 ) ) ;
#2644 = CARTESIAN_POINT ( 'NONE',  ( -125.0000000000002558, -125.0000000000000000, 20.00000000000000000 ) ) ;
#2645 = AXIS2_PLACEMENT_3D ( 'NONE', #1861, #1822, #2537 ) ;
#2646 = DIRECTION ( 'NONE',  ( -0.000000000000000000, 0.000000000000000000, 1.000000000000000000 ) ) ;
#2647 = ORIENTED_EDGE ( 'NONE', *, *, #8043, .T. ) ;
#2648 = DIRECTION ( 'NONE',  ( 1.000000000000000000, 0.000000000000000000, 0.000000000000000000 ) ) ;
#2649 = EDGE_CURVE ( 'NONE', #5704, #6005, #7633, .T. ) ;
#2650 = ORIENTED_EDGE ( 'NONE', *, *, #8282, .F. ) ;
#2651 = ORIENTED_EDGE ( 'NONE', *, *, #6791, .F. ) ;
#2652 = DIRECTION ( 'NONE',  ( 1.000000000000000000, 0.000000000000000000, 0.000000000000000000 ) ) ;
#2653 = AXIS2_PLACEMENT_3D ( 'NONE', #7756, #3895, #2476 ) ;
#2654 = ORIENTED_EDGE ( 'NONE', *, *, #922, .F. ) ;
#2655 = DIRECTION ( 'NONE',  ( -0.000000000000000000, -0.000000000000000000, 1.000000000000000000 ) ) ;
#2656 = CARTESIAN_POINT ( 'NONE',  ( 55.00000000000000711, -75.00000000000000000, -27.50000000000000000 ) ) ;
#2657 = ITEM_DEFINED_TRANSFORMATION ( 'NONE', 'NONE', #7600,  #1299 ) ;
#2658 = FACE_OUTER_BOUND ( 'NONE', #4634, .T. ) ;
#2659 = VECTOR ( 'NONE', #195, 1000.000000000000000 ) ;
#2660 = LINE ( 'NONE', #7974, #2151 ) ;
#2661 = ORIENTED_EDGE ( 'NONE', *, *, #2032, .F. ) ;
#2662 = DIRECTION ( 'NONE',  ( -1.000000000000000000, -0.000000000000000000, -0.000000000000000000 ) ) ;
#2663 = VECTOR ( 'NONE', #3824, 1000.000000000000000 ) ;
#2664 = DIRECTION ( 'NONE',  ( 0.000000000000000000, 0.000000000000000000, 1.000000000000000000 ) ) ;
#2665 = VERTEX_POINT ( 'NONE', #8308 ) ;
#2666 = CIRCLE ( 'NONE', #7389, 12.99999999999999822 ) ;
#2667 = DIRECTION ( 'NONE',  ( 1.000000000000000000, 0.000000000000000000, -0.000000000000000000 ) ) ;
#2668 = CARTESIAN_POINT ( 'NONE',  ( 50.00000000000000711, 55.00000000000000000, 220.0000000000000284 ) ) ;
#2669 = CARTESIAN_POINT ( 'NONE',  ( 5.551115123125782702E-14, 12.49999999999999645, -1.387778780781445676E-14 ) ) ;
#2670 = AXIS2_PLACEMENT_3D ( 'NONE', #7208, #5939, #4628 ) ;
#2671 = CARTESIAN_POINT ( 'NONE',  ( 75.00000000000001421, 9.184850993605150311E-15, 20.00000000000000355 ) ) ;
#2672 = PRODUCT_DEFINITION ( 'UNKNOWN', '', #7994, #233 ) ;
#2673 = CARTESIAN_POINT ( 'NONE',  ( 102.5000000000000000, 0.000000000000000000, 0.000000000000000000 ) ) ;
#2674 = VERTEX_POINT ( 'NONE', #5084 ) ;
#2675 = FACE_OUTER_BOUND ( 'NONE', #4531, .T. ) ;
#2676 = CARTESIAN_POINT ( 'NONE',  ( 2.273222919052576864E-14, 91.25000000000001421, -188.2499999999999147 ) ) ;
#2677 = AXIS2_PLACEMENT_3D ( 'NONE', #4426, #7098, #5199 ) ;
#2678 = ADVANCED_FACE ( 'NONE', ( #3179 ), #5770, .F. ) ;
#2679 = ADVANCED_FACE ( 'NONE', ( #4914 ), #6867, .F. ) ;
#2680 = EDGE_LOOP ( 'NONE', ( #1548, #2626, #5631, #3946 ) ) ;
#2681 = DIRECTION ( 'NONE',  ( -0.000000000000000000, -0.000000000000000000, 1.000000000000000000 ) ) ;
#2682 = VECTOR ( 'NONE', #2330, 1000.000000000000000 ) ;
#2683 = VECTOR ( 'NONE', #4190, 1000.000000000000000 ) ;
#2684 = FACE_OUTER_BOUND ( 'NONE', #4430, .T. ) ;
#2685 = EDGE_CURVE ( 'NONE', #306, #7564, #6522, .T. ) ;
#2686 = AXIS2_PLACEMENT_3D ( 'NONE', #3148, #3792, #6322 ) ;
#2687 = DIRECTION ( 'NONE',  ( -0.000000000000000000, -0.000000000000000000, 1.000000000000000000 ) ) ;
#2688 = ORIENTED_EDGE ( 'NONE', *, *, #6794, .F. ) ;
#2689 = ORIENTED_EDGE ( 'NONE', *, *, #7492, .F. ) ;
#2690 = DIRECTION ( 'NONE',  ( -1.000000000000000000, -1.224646799147353207E-16, 9.730231958057834423E-34 ) ) ;
#2691 = AXIS2_PLACEMENT_3D ( 'NONE', #5259, #3979, #5333 ) ;
#2692 = CIRCLE ( 'NONE', #3349, 12.50000000000000000 ) ;
#2693 = ORIENTED_EDGE ( 'NONE', *, *, #6105, .F. ) ;
#2694 = FACE_OUTER_BOUND ( 'NONE', #3875, .T. ) ;
#2695 = DIRECTION ( 'NONE',  ( -0.000000000000000000, -0.000000000000000000, 1.000000000000000000 ) ) ;
#2696 = ADVANCED_FACE ( 'NONE', ( #2038 ), #1945, .T. ) ;
#2697 = CARTESIAN_POINT ( 'NONE',  ( -55.00000000000000000, 55.00000000000000000, 240.0000000000000284 ) ) ;
#2698 = VECTOR ( 'NONE', #7949, 1000.000000000000000 ) ;
#2699 = CIRCLE ( 'NONE', #808, 5.999999999999991118 ) ;
#2700 = DIRECTION ( 'NONE',  ( 1.000000000000000000, 0.000000000000000000, 0.000000000000000000 ) ) ;
#2701 = ORIENTED_EDGE ( 'NONE', *, *, #3345, .T. ) ;
#2702 = LINE ( 'NONE', #4037, #7554 ) ;
#2703 = FACE_BOUND ( 'NONE', #6143, .T. ) ;
#2704 = CYLINDRICAL_SURFACE ( 'NONE', #6225, 2.499999999999990230 ) ;
#2705 = ORIENTED_EDGE ( 'NONE', *, *, #3419, .T. ) ;
#2706 = CARTESIAN_POINT ( 'NONE',  ( -120.0000000000000000, -120.0000000000000000, 0.000000000000000000 ) ) ;
#2707 = CARTESIAN_POINT ( 'NONE',  ( 120.0000000000000000, 125.0000000000000000, -28.00000000000002487 ) ) ;
#2708 = DIRECTION ( 'NONE',  ( -0.000000000000000000, -0.000000000000000000, 1.000000000000000000 ) ) ;
#2709 = CARTESIAN_POINT ( 'NONE',  ( -125.0000000000000000, 52.49999999999997158, 0.000000000000000000 ) ) ;
#2710 = ORIENTED_EDGE ( 'NONE', *, *, #6560, .T. ) ;
#2711 = DIRECTION ( 'NONE',  ( -1.000000000000000000, 0.000000000000000000, 0.000000000000000000 ) ) ;
#2713 = ORIENTED_EDGE ( 'NONE', *, *, #397, .T. ) ;
#2712 = CIRCLE ( 'NONE', #1586, 9.500000000000008882 ) ;
#2714 = CARTESIAN_POINT ( 'NONE',  ( -105.0000000000000000, 105.0000000000000284, 240.0000000000000284 ) ) ;
#2715 = ADVANCED_FACE ( 'NONE', ( #661 ), #7879, .T. ) ;
#2716 = DIRECTION ( 'NONE',  ( -1.000000000000000000, -0.000000000000000000, -0.000000000000000000 ) ) ;
#2717 = CARTESIAN_POINT ( 'NONE',  ( 55.00000000000000000, -55.00000000000000000, 240.0000000000000284 ) ) ;
#2718 =( LENGTH_UNIT ( ) NAMED_UNIT ( * ) SI_UNIT ( .MILLI., .METRE. ) );
#2719 = DIRECTION ( 'NONE',  ( -0.000000000000000000, -0.000000000000000000, -1.000000000000000000 ) ) ;
#2720 = ORIENTED_EDGE ( 'NONE', *, *, #2079, .T. ) ;
#2721 = ADVANCED_FACE ( 'NONE', ( #746 ), #4484, .F. ) ;
#2722 = CARTESIAN_POINT ( 'NONE',  ( 49.00000000000000000, -55.00000000000000711, 27.50000000000000000 ) ) ;
#2723 = EDGE_CURVE ( 'NONE', #3656, #5338, #5303, .T. ) ;
#2724 = FACE_OUTER_BOUND ( 'NONE', #1464, .T. ) ;
#2725 = ADVANCED_FACE ( 'NONE', ( #7808 ), #7199, .F. ) ;
#2726 = ORIENTED_EDGE ( 'NONE', *, *, #3628, .F. ) ;
#2727 = CARTESIAN_POINT ( 'NONE',  ( -31.74999999999995737, 0.000000000000000000, 0.000000000000000000 ) ) ;
#2728 = ORIENTED_EDGE ( 'NONE', *, *, #3761, .F. ) ;
#2729 = LINE ( 'NONE', #838, #3335 ) ;
#2730 = AXIS2_PLACEMENT_3D ( 'NONE', #4327, #8272, #1853 ) ;
#2731 = LINE ( 'NONE', #752, #7531 ) ;
#2732 = ORIENTED_EDGE ( 'NONE', *, *, #2279, .T. ) ;
#2733 = CARTESIAN_POINT ( 'NONE',  ( 54.99999999999999289, -55.00000000000000711, 27.50000000000000000 ) ) ;
#2734 = EDGE_CURVE ( 'NONE', #1294, #7972, #4807, .T. ) ;
#2735 = VERTEX_POINT ( 'NONE', #2115 ) ;
#2736 = DIRECTION ( 'NONE',  ( -1.000000000000000000, -0.000000000000000000, -0.000000000000000000 ) ) ;
#2737 = CARTESIAN_POINT ( 'NONE',  ( 54.99999999999999289, -54.99999999999999289, 27.50000000000000000 ) ) ;
#2738 = AXIS2_PLACEMENT_3D ( 'NONE', #1503, #2307, #989 ) ;
#2739 = CARTESIAN_POINT ( 'NONE',  ( 5.000000000000000000, 4.685197434473814759, -5.637851296924623057E-15 ) ) ;
#2740 = DIRECTION ( 'NONE',  ( -0.8571673007021116675, 1.049727191138617833E-16, 0.5150380749100552658 ) ) ;
#2741 = DIRECTION ( 'NONE',  ( 1.752490724247363967E-17, -1.000000000000000000, 3.853078496550152365E-17 ) ) ;
#2742 = CARTESIAN_POINT ( 'NONE',  ( -105.0000000000000000, -72.49999999999994316, -212.5000000000000568 ) ) ;
#2743 = PLANE ( 'NONE',  #6305 ) ;
#2744 = CARTESIAN_POINT ( 'NONE',  ( 20.76917701662883076, 5.000000000000000000, 0.000000000000000000 ) ) ;
#2745 = ORIENTED_EDGE ( 'NONE', *, *, #7529, .T. ) ;
#2746 = DIRECTION ( 'NONE',  ( 0.000000000000000000, 1.000000000000000000, -0.000000000000000000 ) ) ;
#2747 = CONICAL_SURFACE ( 'NONE', #5720, 4.999999999999990230, 1.029744258676653201 ) ;
#2748 = EDGE_LOOP ( 'NONE', ( #129, #5296, #1145, #4036 ) ) ;
#2749 = DIRECTION ( 'NONE',  ( 0.000000000000000000, 0.000000000000000000, 1.000000000000000000 ) ) ;
#2750 = AXIS2_PLACEMENT_3D ( 'NONE', #303, #5509, #1628 ) ;
#2751 = LINE ( 'NONE', #7916, #742 ) ;
#2752 = DIRECTION ( 'NONE',  ( 1.000000000000000000, 0.000000000000000000, 0.000000000000000000 ) ) ;
#2753 = FACE_OUTER_BOUND ( 'NONE', #2804, .T. ) ;
#2754 = DIRECTION ( 'NONE',  ( -1.460819769243625652E-16, 1.000000000000000000, 0.000000000000000000 ) ) ;
#2755 = DIRECTION ( 'NONE',  ( -0.000000000000000000, -0.000000000000000000, 1.000000000000000000 ) ) ;
#2756 = PLANE ( 'NONE',  #4396 ) ;
#2757 = EDGE_CURVE ( 'NONE', #8025, #2041, #7241, .T. ) ;
#2758 = ORIENTED_EDGE ( 'NONE', *, *, #240, .F. ) ;
#2759 = CYLINDRICAL_SURFACE ( 'NONE', #3605, 15.00000000000001421 ) ;
#2760 = ORIENTED_EDGE ( 'NONE', *, *, #6371, .F. ) ;
#2761 = EDGE_LOOP ( 'NONE', ( #662, #5308, #3301, #6052 ) ) ;
#2762 = PLANE ( 'NONE',  #6990 ) ;
#2763 = PLANE ( 'NONE',  #4953 ) ;
#2764 = EDGE_CURVE ( 'NONE', #3078, #1537, #7927, .T. ) ;
#2765 = FACE_OUTER_BOUND ( 'NONE', #5148, .T. ) ;
#2766 = CYLINDRICAL_SURFACE ( 'NONE', #2975, 4.999999999999997335 ) ;
#2767 = EDGE_CURVE ( 'NONE', #4692, #7479, #1340, .T. ) ;
#2768 = EDGE_CURVE ( 'NONE', #1436, #3146, #56, .T. ) ;
#2769 = EDGE_CURVE ( 'NONE', #167, #6494, #2792, .T. ) ;
#2770 =( GEOMETRIC_REPRESENTATION_CONTEXT ( 3 ) GLOBAL_UNCERTAINTY_ASSIGNED_CONTEXT ( ( #2208 ) ) GLOBAL_UNIT_ASSIGNED_CONTEXT ( ( #5967, #3298, #4614 ) ) REPRESENTATION_CONTEXT ( 'NONE', 'WORKASPACE' ) );
#2771 = ORIENTED_EDGE ( 'NONE', *, *, #7745, .F. ) ;
#2772 = DIRECTION ( 'NONE',  ( 0.000000000000000000, -1.000000000000000000, 0.000000000000000000 ) ) ;
#2773 = ORIENTED_EDGE ( 'NONE', *, *, #4299, .F. ) ;
#2774 = AXIS2_PLACEMENT_3D ( 'NONE', #2181, #1409, #4730 ) ;
#2775 = CARTESIAN_POINT ( 'NONE',  ( -50.00000000000000000, 55.00000000000000000, 240.0000000000000284 ) ) ;
#2776 = ADVANCED_FACE ( 'NONE', ( #1421 ), #6566, .F. ) ;
#2777 = DIRECTION ( 'NONE',  ( -0.000000000000000000, -7.945337353457666666E-18, -1.000000000000000000 ) ) ;
#2778 =( REPRESENTATION_RELATIONSHIP ('NONE','NONE', #6882, #239 ) REPRESENTATION_RELATIONSHIP_WITH_TRANSFORMATION ( #5738 )SHAPE_REPRESENTATION_RELATIONSHIP( ) );
#2779 = CYLINDRICAL_SURFACE ( 'NONE', #3007, 57.99999999999995737 ) ;
#2780 = PLANE ( 'NONE',  #5358 ) ;
#2781 = AXIS2_PLACEMENT_3D ( 'NONE', #527, #395, #4256 ) ;
#2782 = DIRECTION ( 'NONE',  ( 0.000000000000000000, -1.000000000000000000, -1.460819769243626884E-16 ) ) ;
#2783 = DIRECTION ( 'NONE',  ( 0.000000000000000000, -1.000000000000000000, -1.266875999117951024E-16 ) ) ;
#2784 = CARTESIAN_POINT ( 'NONE',  ( -115.0000000000000000, -115.0000000000000000, 340.0000000000000000 ) ) ;
#2785 = DIRECTION ( 'NONE',  ( 0.000000000000000000, 0.000000000000000000, -1.000000000000000000 ) ) ;
#2786 = ORIENTED_EDGE ( 'NONE', *, *, #4582, .F. ) ;
#2787 = CARTESIAN_POINT ( 'NONE',  ( -104.9999999999999432, -105.0000000000000853, 240.0000000000000284 ) ) ;
#2788 = EDGE_CURVE ( 'NONE', #4729, #1566, #5129, .T. ) ;
#2789 = AXIS2_PLACEMENT_3D ( 'NONE', #2998, #4857, #3721 ) ;
#2790 = AXIS2_PLACEMENT_3D ( 'NONE', #2132, #6541, #763 ) ;
#2791 = VERTEX_POINT ( 'NONE', #7289 ) ;
#2792 = CIRCLE ( 'NONE', #4539, 5.999999999999991118 ) ;
#2793 = FACE_OUTER_BOUND ( 'NONE', #946, .T. ) ;
#2794 = VECTOR ( 'NONE', #2594, 1000.000000000000000 ) ;
#2795 = CARTESIAN_POINT ( 'NONE',  ( -125.0000000000000000, 52.49999999999997158, 0.000000000000000000 ) ) ;
#2796 = AXIS2_PLACEMENT_3D ( 'NONE', #4981, #714, #5818 ) ;
#2797 = CARTESIAN_POINT ( 'NONE',  ( 125.0000000000000000, 120.0000000000000000, 0.000000000000000000 ) ) ;
#2798 = ORIENTED_EDGE ( 'NONE', *, *, #240, .T. ) ;
#2799 = CONICAL_SURFACE ( 'NONE', #8058, 12.50000000000000000, 0.7853981633974560506 ) ;
#2800 = DIRECTION ( 'NONE',  ( -0.000000000000000000, -0.000000000000000000, 1.000000000000000000 ) ) ;
#2801 = AXIS2_PLACEMENT_3D ( 'NONE', #5240, #3928, #6497 ) ;
#2802 = CARTESIAN_POINT ( 'NONE',  ( -115.0000000000000142, 115.0000000000000000, 16.39483628583463570 ) ) ;
#2803 = VERTEX_POINT ( 'NONE', #7962 ) ;
#2804 = EDGE_LOOP ( 'NONE', ( #546, #6753 ) ) ;
#2805 = CARTESIAN_POINT ( 'NONE',  ( -120.0000000000000000, 120.0000000000000000, 0.000000000000000000 ) ) ;
#2806 = CARTESIAN_POINT ( 'NONE',  ( -10.00000000000000000, 57.99999999999990052, 93.75000000000004263 ) ) ;
#2807 = CIRCLE ( 'NONE', #5241, 5.000000000000004441 ) ;
#2808 = VECTOR ( 'NONE', #2456, 999.9999999999998863 ) ;
#2809 = CARTESIAN_POINT ( 'NONE',  ( 114.9999999999999147, 99.99999999999998579, 250.0000000000000000 ) ) ;
#2810 = DIRECTION ( 'NONE',  ( 0.000000000000000000, 0.000000000000000000, 1.000000000000000000 ) ) ;
#2811 = AXIS2_PLACEMENT_3D ( 'NONE', #2084, #712, #2046 ) ;
#2812 = EDGE_LOOP ( 'NONE', ( #667, #273, #7246, #5388 ) ) ;
#2813 = LINE ( 'NONE', #720, #7936 ) ;
#2814 = ORIENTED_EDGE ( 'NONE', *, *, #2484, .F. ) ;
#2815 = EDGE_CURVE ( 'NONE', #2961, #321, #1509, .T. ) ;
#2816 = FACE_OUTER_BOUND ( 'NONE', #3661, .T. ) ;
#2817 = LINE ( 'NONE', #1565, #4522 ) ;
#2818 = CIRCLE ( 'NONE', #7413, 5.999999999999991118 ) ;
#2819 = AXIS2_PLACEMENT_3D ( 'NONE', #6539, #3393, #3314 ) ;
#2820 = CARTESIAN_POINT ( 'NONE',  ( 8.554558110533218240, 49.26362287191481926, -3.376715202643651992 ) ) ;
#2821 = DIRECTION ( 'NONE',  ( -0.000000000000000000, -0.000000000000000000, 1.000000000000000000 ) ) ;
#2822 = EDGE_CURVE ( 'NONE', #14, #6508, #995, .T. ) ;
#2823 = CARTESIAN_POINT ( 'NONE',  ( 109.5000000000000142, -114.9999999999999716, 0.000000000000000000 ) ) ;
#2824 = AXIS2_PLACEMENT_3D ( 'NONE', #2000, #8279, #4534 ) ;
#2825 = PLANE ( 'NONE',  #1536 ) ;
#2826 = ADVANCED_FACE ( 'NONE', ( #6650 ), #4060, .F. ) ;
#2827 = DIRECTION ( 'NONE',  ( -0.000000000000000000, -0.000000000000000000, 1.000000000000000000 ) ) ;
#2828 = EDGE_CURVE ( 'NONE', #4917, #2993, #913, .T. ) ;
#2829 = CARTESIAN_POINT ( 'NONE',  ( -60.99999999999998579, 55.00000000000000711, 27.50000000000000000 ) ) ;
#2830 = B_SPLINE_CURVE_WITH_KNOTS ( 'NONE', 3,
 ( #1043, #3597, #401, #7500, #4263, #6264, #3644, #1770, #702, #5767, #2643, #2486, #5683, #2563, #658, #4481, #533, #7033, #6353, #1896, #4352, #6426, #618, #5126, #7071, #3258, #3218, #1846, #5848, #5081, #7116, #3177, #5212, #575, #3784, #1171, #5809, #7726, #3736, #7631, #3106, #7764, #6313, #5043, #8266, #4440, #4391, #3860 ),
 .UNSPECIFIED., .F., .F.,
 ( 4, 2, 2, 2, 2, 2, 2, 2, 2, 2, 2, 2, 2, 2, 2, 2, 2, 2, 2, 2, 2, 2, 2, 4 ),
 ( 0.03923685324657889828, 0.04168849572278653104, 0.04414013819899415686, 0.04536595943709797324, 0.04659178067520178962, 0.04904342315140942932, 0.05026924438951324570, 0.05149506562761706902, 0.05394670810382472259, 0.05517252934192855285, 0.05639835058003237617, 0.05762417181813619949, 0.05884999305624002280, 0.06130163553244767638, 0.06375327800865532302, 0.06620492048486296965, 0.06743074172296678603, 0.06865656296107061629, 0.06988238419917444655, 0.07110820543727826293, 0.07355984791348590957, 0.07478566915158973982, 0.07601149038969357008, 0.07846313286590121672 ),
 .UNSPECIFIED. ) ;
#2831 = ORIENTED_EDGE ( 'NONE', *, *, #6813, .F. ) ;
#2832 = EDGE_LOOP ( 'NONE', ( #4045, #7731 ) ) ;
#2833 = ORIENTED_EDGE ( 'NONE', *, *, #8208, .T. ) ;
#2834 = DIRECTION ( 'NONE',  ( 0.000000000000000000, 0.000000000000000000, 1.000000000000000000 ) ) ;
#2835 = EDGE_CURVE ( 'NONE', #6124, #8026, #3416, .T. ) ;
#2836 = EDGE_CURVE ( 'NONE', #5161, #4485, #6155, .T. ) ;
#2837 = DIRECTION ( 'NONE',  ( 0.8571673007021116675, 0.000000000000000000, 0.5150380749100552658 ) ) ;
#2838 = DIRECTION ( 'NONE',  ( -1.000000000000000000, 0.000000000000000000, 0.000000000000000000 ) ) ;
#2839 = CYLINDRICAL_SURFACE ( 'NONE', #2750, 12.99999999999999822 ) ;
#2840 = CARTESIAN_POINT ( 'NONE',  ( -114.9999999999999858, -114.9999999999999858, 20.00000000000000000 ) ) ;
#2841 = EDGE_LOOP ( 'NONE', ( #3155, #883, #6890, #833 ) ) ;
#2842 = CARTESIAN_POINT ( 'NONE',  ( -105.9999999999999858, 114.9999999999999858, 20.00000000000000000 ) ) ;
#2843 = CARTESIAN_POINT ( 'NONE',  ( 0.000000000000000000, -105.0000000000000711, 66.99999999999997158 ) ) ;
#2844 = ORIENTED_EDGE ( 'NONE', *, *, #1046, .F. ) ;
#2845 = CARTESIAN_POINT ( 'NONE',  ( 20.76917701662883076, 5.000000000000000000, 57.99999999999999289 ) ) ;
#2846 = CARTESIAN_POINT ( 'NONE',  ( 0.000000000000000000, 125.0000000000000568, 66.99999999999992895 ) ) ;
#2847 = CARTESIAN_POINT ( 'NONE',  ( 80.00000000000000000, 0.000000000000000000, 0.000000000000000000 ) ) ;
#2848 = CARTESIAN_POINT ( 'NONE',  ( -102.5000000000000000, 0.000000000000000000, 0.000000000000000000 ) ) ;
#2849 = AXIS2_PLACEMENT_3D ( 'NONE', #5425, #7291, #1466 ) ;
#2850 = UNCERTAINTY_MEASURE_WITH_UNIT (LENGTH_MEASURE( 1.000000000000000082E-05 ), #2311, 'distance_accuracy_value', 'NONE');
#2851 = EDGE_LOOP ( 'NONE', ( #708, #2720, #2956, #6617 ) ) ;
#2852 = DIRECTION ( 'NONE',  ( -0.000000000000000000, -0.000000000000000000, 1.000000000000000000 ) ) ;
#2853 = VERTEX_POINT ( 'NONE', #6768 ) ;
#2854 = LINE ( 'NONE', #1097, #2159 ) ;
#2855 =( NAMED_UNIT ( * ) SI_UNIT ( $, .STERADIAN. ) SOLID_ANGLE_UNIT ( ) );
#2856 = EDGE_LOOP ( 'NONE', ( #7495, #6405, #5755, #3429 ) ) ;
#2857 = CARTESIAN_POINT ( 'NONE',  ( -110.0000000000000142, -115.0000000000000000, 340.0000000000000000 ) ) ;
#2858 = AXIS2_PLACEMENT_3D ( 'NONE', #247, #544, #4273 ) ;
#2859 = AXIS2_PLACEMENT_3D ( 'NONE', #2599, #6347, #5163 ) ;
#2860 = EDGE_CURVE ( 'NONE', #3924, #4162, #2014, .T. ) ;
#2861 = FACE_OUTER_BOUND ( 'NONE', #2294, .T. ) ;
#2862 = DIRECTION ( 'NONE',  ( -0.8571673007021134438, 1.049727191138620051E-16, 0.5150380749100522682 ) ) ;
#2863 = DIRECTION ( 'NONE',  ( 1.000000000000000000, 0.000000000000000000, 0.000000000000000000 ) ) ;
#2864 = ORIENTED_EDGE ( 'NONE', *, *, #4321, .F. ) ;
#2865 = EDGE_CURVE ( 'NONE', #2040, #7952, #4139, .T. ) ;
#2866 = EDGE_CURVE ( 'NONE', #7449, #5396, #6705, .T. ) ;
#2867 = AXIS2_PLACEMENT_3D ( 'NONE', #7664, #5113, #1246 ) ;
#2868 = EDGE_CURVE ( 'NONE', #7656, #323, #1547, .T. ) ;
#2869 = ORIENTED_EDGE ( 'NONE', *, *, #7051, .F. ) ;
#2870 = CYLINDRICAL_SURFACE ( 'NONE', #7663, 4.999999999999990230 ) ;
#2871 = DIRECTION ( 'NONE',  ( 1.000000000000000000, -0.000000000000000000, 0.000000000000000000 ) ) ;
#2872 = CIRCLE ( 'NONE', #5037, 12.99999999999999822 ) ;
#2873 = ORIENTED_EDGE ( 'NONE', *, *, #5607, .T. ) ;
#2874 = CARTESIAN_POINT ( 'NONE',  ( -120.9999999999999005, -115.0000000000000000, 8.205133554287239938E-16 ) ) ;
#2875 = LINE ( 'NONE', #908, #4393 ) ;
#2876 = VERTEX_POINT ( 'NONE', #305 ) ;
#2877 = CARTESIAN_POINT ( 'NONE',  ( 0.000000000000000000, 0.000000000000000000, 15.00000000000000000 ) ) ;
#2878 = AXIS2_PLACEMENT_3D ( 'NONE', #6082, #4777, #6611 ) ;
#2879 = COLOUR_RGB ( '',0.7921568627450980005, 0.8196078431372548767, 0.9333333333333333481 ) ;
#2880 = CARTESIAN_POINT ( 'NONE',  ( 105.0000000000000000, 8.487013464091010249E-14, 20.00000000000001776 ) ) ;
#2881 = ORIENTED_EDGE ( 'NONE', *, *, #4940, .T. ) ;
#2882 = LINE ( 'NONE', #4145, #4283 ) ;
#2883 = CARTESIAN_POINT ( 'NONE',  ( -54.99999999999999289, -54.99999999999999289, -27.50000000000000000 ) ) ;
#2884 = PRODUCT ( 'MAT-045', 'MAT-045', '', ( #2257 ) ) ;
#2885 = DIRECTION ( 'NONE',  ( 1.000000000000000000, 0.000000000000000000, 0.000000000000000000 ) ) ;
#2886 =( REPRESENTATION_RELATIONSHIP ('NONE','NONE', #6882, #7203 ) REPRESENTATION_RELATIONSHIP_WITH_TRANSFORMATION ( #1824 )SHAPE_REPRESENTATION_RELATIONSHIP( ) );
#2887 = EDGE_CURVE ( 'NONE', #48, #7126, #2875, .T. ) ;
#2888 = EDGE_LOOP ( 'NONE', ( #6207, #3803, #4865, #5544 ) ) ;
#2889 = ORIENTED_EDGE ( 'NONE', *, *, #4569, .T. ) ;
#2890 = FACE_BOUND ( 'NONE', #8086, .T. ) ;
#2891 = ORIENTED_EDGE ( 'NONE', *, *, #8219, .T. ) ;
#2892 = CARTESIAN_POINT ( 'NONE',  ( 115.0000000000000000, -114.9999999999999716, 10.00000000000000000 ) ) ;
#2893 = CARTESIAN_POINT ( 'NONE',  ( -114.9999999999999574, -115.0000000000000568, -1.599999999999995426 ) ) ;
#2894 = CARTESIAN_POINT ( 'NONE',  ( 54.99999999999999289, 55.00000000000000711, 27.50000000000000000 ) ) ;
#2895 = ORIENTED_EDGE ( 'NONE', *, *, #2822, .F. ) ;
#2896 = CARTESIAN_POINT ( 'NONE',  ( 4.420576121828488247, 49.80565028682020312, -0.8005904993895475164 ) ) ;
#2897 = DIRECTION ( 'NONE',  ( 6.106226635438364917E-16, 3.154042683594196846E-17, 1.000000000000000000 ) ) ;
#2898 = CARTESIAN_POINT ( 'NONE',  ( 0.000000000000000000, -52.49999999999996447, 79.99999999999995737 ) ) ;
#2899 = FACE_OUTER_BOUND ( 'NONE', #2680, .T. ) ;
#2900 = CARTESIAN_POINT ( 'NONE',  ( 15.00000000000000355, 0.000000000000000000, -118.0000000000000284 ) ) ;
#2901=STYLED_ITEM('',(#8393),#3583);
#2902 = ORIENTED_EDGE ( 'NONE', *, *, #180, .T. ) ;
#2903 = CARTESIAN_POINT ( 'NONE',  ( 120.9999999999999005, 115.0000000000000000, 8.205133554287239938E-16 ) ) ;
#2904 = CIRCLE ( 'NONE', #5747, 5.999999999999991118 ) ;
#2905 = ORIENTED_EDGE ( 'NONE', *, *, #2348, .F. ) ;
#2906 = VERTEX_POINT ( 'NONE', #6731 ) ;
#2907 = ORIENTED_EDGE ( 'NONE', *, *, #4580, .F. ) ;
#2908 = VECTOR ( 'NONE', #8122, 1000.000000000000000 ) ;
#2909 = PLANE ( 'NONE',  #1047 ) ;
#2910 = PRODUCT_DEFINITION ( 'UNKNOWN', '', #4750, #4112 ) ;
#2911 = DIRECTION ( 'NONE',  ( 1.000000000000000000, 0.000000000000000000, 0.000000000000000000 ) ) ;
#2912 = EDGE_CURVE ( 'NONE', #1207, #153, #6699, .T. ) ;
#2913 = ORIENTED_EDGE ( 'NONE', *, *, #767, .T. ) ;
#2914 = FILL_AREA_STYLE_COLOUR ( '', #537 ) ;
#2915 = EDGE_CURVE ( 'NONE', #1143, #426, #780, .T. ) ;
#2916 = AXIS2_PLACEMENT_3D ( 'NONE', #2143, #781, #3334 ) ;
#2917 = VECTOR ( 'NONE', #1174, 1000.000000000000000 ) ;
#2918 = VERTEX_POINT ( 'NONE', #959 ) ;
#2919 = CARTESIAN_POINT ( 'NONE',  ( 0.000000000000000000, -72.50000000000000000, 240.0000000000000284 ) ) ;
#2920 = FACE_BOUND ( 'NONE', #5205, .T. ) ;
#2921 = DIRECTION ( 'NONE',  ( -0.000000000000000000, -0.000000000000000000, 1.000000000000000000 ) ) ;
#2922 = CARTESIAN_POINT ( 'NONE',  ( 0.000000000000000000, 0.000000000000000000, 35.00000000000000000 ) ) ;
#2923 = ORIENTED_EDGE ( 'NONE', *, *, #7157, .T. ) ;
#2924 = DIRECTION ( 'NONE',  ( -0.000000000000000000, -0.000000000000000000, 1.000000000000000000 ) ) ;
#2925 = EDGE_CURVE ( 'NONE', #15, #6775, #7123, .T. ) ;
#2926 = ADVANCED_FACE ( 'NONE', ( #1629, #5970 ), #2756, .T. ) ;
#2927 = LINE ( 'NONE', #5519, #4384 ) ;
#2928 = ORIENTED_EDGE ( 'NONE', *, *, #2183, .F. ) ;
#2929 =( LENGTH_UNIT ( ) NAMED_UNIT ( * ) SI_UNIT ( .MILLI., .METRE. ) );
#2930 = CIRCLE ( 'NONE', #3460, 15.00000000000000178 ) ;
#2931 = CARTESIAN_POINT ( 'NONE',  ( -125.0000000000000000, 125.0000000000000000, 340.0000000000000000 ) ) ;
#2932 = VECTOR ( 'NONE', #1399, 1000.000000000000000 ) ;
#2933 = PRODUCT_DEFINITION_CONTEXT ( 'detailed design', #5219, 'design' ) ;
#2934 = ORIENTED_EDGE ( 'NONE', *, *, #152, .F. ) ;
#2935 = CARTESIAN_POINT ( 'NONE',  ( 25.00000000000000000, 3.061616997868383043E-15, -126.0000000000000284 ) ) ;
#2936 = AXIS2_PLACEMENT_3D ( 'NONE', #276, #1141, #5484 ) ;
#2937 = AXIS2_PLACEMENT_3D ( 'NONE', #7638, #4399, #5778 ) ;
#2938 = EDGE_LOOP ( 'NONE', ( #623, #5176, #3760, #4346 ) ) ;
#2939 = DIRECTION ( 'NONE',  ( 1.000000000000000000, 0.000000000000000000, 0.000000000000000000 ) ) ;
#2940 = ADVANCED_FACE ( 'NONE', ( #2137 ), #2743, .T. ) ;
#2941 = ORIENTED_EDGE ( 'NONE', *, *, #5514, .F. ) ;
#2942 = APPLICATION_PROTOCOL_DEFINITION ( 'draft international standard', 'automotive_design', 1998, #5106 ) ;
#2943 = ORIENTED_EDGE ( 'NONE', *, *, #5416, .F. ) ;
#2944 = CARTESIAN_POINT ( 'NONE',  ( 0.8294483708339475125, 49.99999999999998579, -1.039817646049378781E-14 ) ) ;
#2945 = ORIENTED_EDGE ( 'NONE', *, *, #3376, .F. ) ;
#2946 = DIRECTION ( 'NONE',  ( -0.000000000000000000, -0.000000000000000000, 1.000000000000000000 ) ) ;
#2947 = DIRECTION ( 'NONE',  ( -0.000000000000000000, -0.000000000000000000, -1.000000000000000000 ) ) ;
#2948 = VERTEX_POINT ( 'NONE', #5291 ) ;
#2949 = DIRECTION ( 'NONE',  ( 0.000000000000000000, 0.000000000000000000, -1.000000000000000000 ) ) ;
#2950 = VECTOR ( 'NONE', #2716, 1000.000000000000000 ) ;
#2951 = AXIS2_PLACEMENT_3D ( 'NONE', #8328, #7050, #5827 ) ;
#2952 = VERTEX_POINT ( 'NONE', #7185 ) ;
#2953 = CARTESIAN_POINT ( 'NONE',  ( -125.0000000000002558, -125.0000000000000000, 20.00000000000000000 ) ) ;
#2954 = EDGE_LOOP ( 'NONE', ( #1372, #2329, #4010, #542 ) ) ;
#2955 = AXIS2_PLACEMENT_3D ( 'NONE', #6274, #7509, #7986 ) ;
#2956 = ORIENTED_EDGE ( 'NONE', *, *, #6806, .T. ) ;
#2957 = CYLINDRICAL_SURFACE ( 'NONE', #4804, 5.499999999999991118 ) ;
#2958 = CARTESIAN_POINT ( 'NONE',  ( 0.000000000000000000, -105.0000000000000711, 79.99999999999997158 ) ) ;
#2959 = ORIENTED_EDGE ( 'NONE', *, *, #1556, .F. ) ;
#2960 =( NAMED_UNIT ( * ) SI_UNIT ( $, .STERADIAN. ) SOLID_ANGLE_UNIT ( ) );
#2961 = VERTEX_POINT ( 'NONE', #7273 ) ;
#2962 = CARTESIAN_POINT ( 'NONE',  ( -15.00000000000000000, 1.836970198721029589E-15, -128.0000000000000284 ) ) ;
#2963 = ADVANCED_FACE ( 'NONE', ( #3970 ), #7224, .F. ) ;
#2964 = EDGE_CURVE ( 'NONE', #6525, #4104, #3083, .T. ) ;
#2965 = LINE ( 'NONE', #4950, #7512 ) ;
#2966 = CARTESIAN_POINT ( 'NONE',  ( -1.110223024625156540E-13, -12.50000000000001066, 1.387778780781445676E-14 ) ) ;
#2967 = AXIS2_PLACEMENT_3D ( 'NONE', #4370, #3835, #6926 ) ;
#2968 = EDGE_LOOP ( 'NONE', ( #5843, #2498, #7900, #4205 ) ) ;
#2969 = DIRECTION ( 'NONE',  ( -0.000000000000000000, -0.000000000000000000, 1.000000000000000000 ) ) ;
#2970 = ORIENTED_EDGE ( 'NONE', *, *, #3484, .T. ) ;
#2971 = DIRECTION ( 'NONE',  ( -0.000000000000000000, -7.945337353457666666E-18, -1.000000000000000000 ) ) ;
#2972 = CARTESIAN_POINT ( 'NONE',  ( 60.00000000000000000, 55.00000000000000000, 240.0000000000000284 ) ) ;
#2973 = EDGE_LOOP ( 'NONE', ( #424, #2365 ) ) ;
#2974 = CARTESIAN_POINT ( 'NONE',  ( 10.00000000000000000, -3.448762466456902719E-14, 93.74999999999998579 ) ) ;
#2975 = AXIS2_PLACEMENT_3D ( 'NONE', #2049, #4031, #5898 ) ;
#2976 = EDGE_CURVE ( 'NONE', #7110, #8191, #5228, .T. ) ;
#2977 = EDGE_CURVE ( 'NONE', #1656, #3598, #1330, .T. ) ;
#2978 = ORIENTED_EDGE ( 'NONE', *, *, #664, .T. ) ;
#2979 = DIRECTION ( 'NONE',  ( 0.000000000000000000, 0.000000000000000000, -1.000000000000000000 ) ) ;
#2980 = ORIENTED_EDGE ( 'NONE', *, *, #6601, .T. ) ;
#2981 = CARTESIAN_POINT ( 'NONE',  ( 10.00000000000000000, 57.99999999999990052, 93.75000000000004263 ) ) ;
#2982 = LINE ( 'NONE', #3658, #2570 ) ;
#2983 = ORIENTED_EDGE ( 'NONE', *, *, #6855, .T. ) ;
#2984 = PRODUCT_CONTEXT ( 'NONE', #6112, 'mechanical' ) ;
#2985 = ORIENTED_EDGE ( 'NONE', *, *, #241, .F. ) ;
#2986 = CARTESIAN_POINT ( 'NONE',  ( 115.0000000000000000, 115.0000000000000000, 20.00000000000000355 ) ) ;
#2987 = ORIENTED_EDGE ( 'NONE', *, *, #840, .T. ) ;
#2988 = CARTESIAN_POINT ( 'NONE',  ( 1.562058576037991531E-17, 0.000000000000000000, 0.000000000000000000 ) ) ;
#2989 = VECTOR ( 'NONE', #1568, 1000.000000000000000 ) ;
#2990 = FACE_OUTER_BOUND ( 'NONE', #6141, .T. ) ;
#2991 = ORIENTED_EDGE ( 'NONE', *, *, #5537, .F. ) ;
#2992 = CARTESIAN_POINT ( 'NONE',  ( 55.00000000000000711, 75.00000000000000000, 27.50000000000000000 ) ) ;
#2993 = VERTEX_POINT ( 'NONE', #5021 ) ;
#2994 = ORIENTED_EDGE ( 'NONE', *, *, #2887, .F. ) ;
#2995 = DIRECTION ( 'NONE',  ( 1.000000000000000000, 0.000000000000000000, 0.000000000000000000 ) ) ;
#2996 = ORIENTED_EDGE ( 'NONE', *, *, #308, .T. ) ;
#2997 = DIRECTION ( 'NONE',  ( -0.000000000000000000, -0.000000000000000000, 1.000000000000000000 ) ) ;
#2998 = CARTESIAN_POINT ( 'NONE',  ( -120.0000000000000000, -120.0000000000000000, -28.00000000000002487 ) ) ;
#2999 = FACE_OUTER_BOUND ( 'NONE', #5824, .T. ) ;
#3000 = VERTEX_POINT ( 'NONE', #6287 ) ;
#3001 = CARTESIAN_POINT ( 'NONE',  ( 0.000000000000000000, -49.99999999999999289, 0.000000000000000000 ) ) ;
#3002 = VECTOR ( 'NONE', #7020, 1000.000000000000000 ) ;
#3003 = FILL_AREA_STYLE ('',( #1079 ) ) ;
#3004 = ORIENTED_EDGE ( 'NONE', *, *, #5828, .T. ) ;
#3005 = CARTESIAN_POINT ( 'NONE',  ( 0.000000000000000000, 125.0000000000000000, -12.50000000000000000 ) ) ;
#3006 = DIRECTION ( 'NONE',  ( 0.000000000000000000, 1.000000000000000000, 0.000000000000000000 ) ) ;
#3007 = AXIS2_PLACEMENT_3D ( 'NONE', #5359, #3440, #2421 ) ;
#3008 = FACE_OUTER_BOUND ( 'NONE', #5304, .T. ) ;
#3009 = ORIENTED_EDGE ( 'NONE', *, *, #1556, .T. ) ;
#3010 = CARTESIAN_POINT ( 'NONE',  ( 75.00000000000001421, 9.184850993605150311E-15, 0.000000000000000000 ) ) ;
#3011 = DIRECTION ( 'NONE',  ( 0.000000000000000000, -2.960594732333750117E-16, 1.000000000000000000 ) ) ;
#3012 = ADVANCED_FACE ( 'NONE', ( #63 ), #468, .F. ) ;
#3013 = DIRECTION ( 'NONE',  ( 0.000000000000000000, 0.000000000000000000, 1.000000000000000000 ) ) ;
#3014=STYLED_ITEM('',(#8393),#706);
#3015 = VERTEX_POINT ( 'NONE', #2467 ) ;
#3016 = EDGE_LOOP ( 'NONE', ( #3304, #7912 ) ) ;
#3017 = FACE_OUTER_BOUND ( 'NONE', #8250, .T. ) ;
#3018 = CARTESIAN_POINT ( 'NONE',  ( 125.0000000000000000, 125.0000000000000000, 340.0000000000000000 ) ) ;
#3019 = ORIENTED_EDGE ( 'NONE', *, *, #5206, .T. ) ;
#3020 = DIRECTION ( 'NONE',  ( 0.000000000000000000, 0.000000000000000000, -1.000000000000000000 ) ) ;
#3021 = FACE_OUTER_BOUND ( 'NONE', #5891, .T. ) ;
#3022 = EDGE_CURVE ( 'NONE', #6613, #1534, #5582, .T. ) ;
#3023 = EDGE_LOOP ( 'NONE', ( #1553, #6192, #1782, #6408 ) ) ;
#3024 = EDGE_CURVE ( 'NONE', #2876, #8288, #7254, .T. ) ;
#3025 = ADVANCED_FACE ( 'NONE', ( #7522 ), #4933, .F. ) ;
#3026 = CARTESIAN_POINT ( 'NONE',  ( 0.000000000000000000, 0.000000000000000000, -128.0000000000000284 ) ) ;
#3027 = DIRECTION ( 'NONE',  ( -1.000000000000000000, 0.000000000000000000, 0.000000000000000000 ) ) ;
#3028 = PRODUCT_DEFINITION_SHAPE ( 'NONE', 'NONE',  #8348 ) ;
#3029 = ORIENTED_EDGE ( 'NONE', *, *, #6750, .F. ) ;
#3030 = CARTESIAN_POINT ( 'NONE',  ( 4.999999999999994671, 0.000000000000000000, 0.000000000000000000 ) ) ;
#3031 = EDGE_LOOP ( 'NONE', ( #2568, #5226, #7519, #4754 ) ) ;
#3032 = ORIENTED_EDGE ( 'NONE', *, *, #3319, .F. ) ;
#3033 = CARTESIAN_POINT ( 'NONE',  ( 109.5000000000000142, 114.9999999999999716, 0.000000000000000000 ) ) ;
#3034 = DIRECTION ( 'NONE',  ( -0.000000000000000000, -1.000000000000000000, 1.586032892321652236E-16 ) ) ;
#3035 = ADVANCED_FACE ( 'NONE', ( #1302 ), #6484, .T. ) ;
#3036 = EDGE_CURVE ( 'NONE', #3698, #372, #7673, .T. ) ;
#3037 = EDGE_LOOP ( 'NONE', ( #85, #2978, #5901, #521 ) ) ;
#3038 = ORIENTED_EDGE ( 'NONE', *, *, #3430, .T. ) ;
#3039 = ORIENTED_EDGE ( 'NONE', *, *, #2471, .T. ) ;
#3040 = AXIS2_PLACEMENT_3D ( 'NONE', #5707, #2591, #7660 ) ;
#3041 = LINE ( 'NONE', #6848, #6424 ) ;
#3042 = DIRECTION ( 'NONE',  ( -0.000000000000000000, -0.000000000000000000, 1.000000000000000000 ) ) ;
#3043 = DIRECTION ( 'NONE',  ( 0.000000000000000000, 1.000000000000000000, 1.224646799147353207E-16 ) ) ;
#3044 = VERTEX_POINT ( 'NONE', #2047 ) ;
#3045 = EDGE_CURVE ( 'NONE', #4012, #7120, #1999, .T. ) ;
#3046 = CARTESIAN_POINT ( 'NONE',  ( -7.630101673356672443, -49.41909675622684261, -22.43442449636368607 ) ) ;
#3047 = AXIS2_PLACEMENT_3D ( 'NONE', #4343, #1251, #7105 ) ;
#3048 = EDGE_LOOP ( 'NONE', ( #3831, #2798 ) ) ;
#3049 = CARTESIAN_POINT ( 'NONE',  ( -109.0000000000000142, 115.0000000000000000, 20.00000000000000355 ) ) ;
#3050 =( REPRESENTATION_RELATIONSHIP ('NONE','NONE', #6882, #239 ) REPRESENTATION_RELATIONSHIP_WITH_TRANSFORMATION ( #24 )SHAPE_REPRESENTATION_RELATIONSHIP( ) );
#3051 = PLANE ( 'NONE',  #945 ) ;
#3052 = ORIENTED_EDGE ( 'NONE', *, *, #6423, .F. ) ;
#3053 = CONICAL_SURFACE ( 'NONE', #1318, 4.999999999999990230, 1.029744258676656754 ) ;
#3054 = ORIENTED_EDGE ( 'NONE', *, *, #2268, .F. ) ;
#3055 = CYLINDRICAL_SURFACE ( 'NONE', #6596, 20.00000000000000355 ) ;
#3056 = DIRECTION ( 'NONE',  ( -0.000000000000000000, -0.000000000000000000, 1.000000000000000000 ) ) ;
#3057 = AXIS2_PLACEMENT_3D ( 'NONE', #7415, #4822, #4743 ) ;
#3058 = PLANE ( 'NONE',  #3876 ) ;
#3059 = CIRCLE ( 'NONE', #5079, 4.999999999999990230 ) ;
#3060 = EDGE_LOOP ( 'NONE', ( #1041, #1105 ) ) ;
#3061 = VECTOR ( 'NONE', #6083, 1000.000000000000000 ) ;
#3062 = ORIENTED_EDGE ( 'NONE', *, *, #5281, .F. ) ;
#3063 = DIRECTION ( 'NONE',  ( 0.000000000000000000, -0.000000000000000000, -1.000000000000000000 ) ) ;
#3064 = FACE_OUTER_BOUND ( 'NONE', #4958, .T. ) ;
#3065 = VERTEX_POINT ( 'NONE', #1111 ) ;
#3066 = CARTESIAN_POINT ( 'NONE',  ( 80.00000000000000000, 0.000000000000000000, 4.171999999999999709 ) ) ;
#3067 = FACE_OUTER_BOUND ( 'NONE', #5317, .T. ) ;
#3068 = AXIS2_PLACEMENT_3D ( 'NONE', #2422, #7395, #5617 ) ;
#3069 = VERTEX_POINT ( 'NONE', #6440 ) ;
#3070 = SHAPE_DEFINITION_REPRESENTATION ( #813, #8061 ) ;
#3071 = VECTOR ( 'NONE', #2695, 1000.000000000000000 ) ;
#3072 = VERTEX_POINT ( 'NONE', #3670 ) ;
#3073 = CARTESIAN_POINT ( 'NONE',  ( 3.257728639534230197, 49.90026920665918198, -24.59591892738197672 ) ) ;
#3074 = ADVANCED_FACE ( 'NONE', ( #674 ), #7169, .F. ) ;
#3075 = FACE_BOUND ( 'NONE', #3160, .T. ) ;
#3076 = VECTOR ( 'NONE', #2120, 1000.000000000000000 ) ;
#3077 = VECTOR ( 'NONE', #4228, 1000.000000000000227 ) ;
#3078 = VERTEX_POINT ( 'NONE', #4533 ) ;
#3079 = EDGE_CURVE ( 'NONE', #5024, #3849, #8246, .T. ) ;
#3080 = LINE ( 'NONE', #5662, #6442 ) ;
#3081 = ORIENTED_EDGE ( 'NONE', *, *, #3910, .F. ) ;
#3082 = CYLINDRICAL_SURFACE ( 'NONE', #2169, 5.999999999999991118 ) ;
#3083 = LINE ( 'NONE', #3231, #8055 ) ;
#3084 = DIRECTION ( 'NONE',  ( -1.000000000000000000, 0.000000000000000000, 0.000000000000000000 ) ) ;
#3085 = CIRCLE ( 'NONE', #1892, 5.499999999999991118 ) ;
#3086 = VECTOR ( 'NONE', #7343, 1000.000000000000000 ) ;
#3087 = CARTESIAN_POINT ( 'NONE',  ( -10.16604137791875750, 48.95616179457642403, -5.215114234092023793 ) ) ;
#3088 = ORIENTED_EDGE ( 'NONE', *, *, #1025, .F. ) ;
#3089 = EDGE_CURVE ( 'NONE', #5894, #5749, #1389, .T. ) ;
#3090 = CARTESIAN_POINT ( 'NONE',  ( 10.00000000000000000, 57.99999999999997868, -93.74999999999997158 ) ) ;
#3091 = VECTOR ( 'NONE', #3374, 1000.000000000000000 ) ;
#3092 = CIRCLE ( 'NONE', #4565, 4.999999999999997335 ) ;
#3093 = CYLINDRICAL_SURFACE ( 'NONE', #4287, 9.000000000000007105 ) ;
#3094 = VERTEX_POINT ( 'NONE', #2656 ) ;
#3095 = CARTESIAN_POINT ( 'NONE',  ( -10.82421258667007891, -48.81470695058813902, -18.76526308057255932 ) ) ;
#3096 = DIRECTION ( 'NONE',  ( 1.000000000000000000, 0.000000000000000000, 0.000000000000000000 ) ) ;
#3097 = CIRCLE ( 'NONE', #3485, 15.00000000000001421 ) ;
#3098 = VECTOR ( 'NONE', #6758, 1000.000000000000000 ) ;
#3099 = LINE ( 'NONE', #5718, #4248 ) ;
#3100 = ORIENTED_EDGE ( 'NONE', *, *, #6902, .F. ) ;
#3101 = VECTOR ( 'NONE', #1685, 1000.000000000000000 ) ;
#3102 = CARTESIAN_POINT ( 'NONE',  ( 17.61817604250836311, 0.000000000000000000, -120.5000000000000284 ) ) ;
#3103 = ADVANCED_FACE ( 'NONE', ( #7818 ), #1790, .F. ) ;
#3104 = CARTESIAN_POINT ( 'NONE',  ( 55.00000000000000000, 55.00000000000000000, 240.0000000000000284 ) ) ;
#3105 = DIRECTION ( 'NONE',  ( 0.000000000000000000, 0.000000000000000000, -1.000000000000000000 ) ) ;
#3106 = CARTESIAN_POINT ( 'NONE',  ( 5.558076868459242981, -49.69586384218322905, -1.274058936613802651 ) ) ;
#3107 = CARTESIAN_POINT ( 'NONE',  ( -10.00000000000000000, -58.00000000000000711, 93.74999999999998579 ) ) ;
#3108 = CARTESIAN_POINT ( 'NONE',  ( -95.00000000000000000, 95.00000000000008527, 70.00000000000000000 ) ) ;
#3109 = ORIENTED_EDGE ( 'NONE', *, *, #4431, .F. ) ;
#3110 = UNCERTAINTY_MEASURE_WITH_UNIT (LENGTH_MEASURE( 1.000000000000000082E-05 ), #2351, 'distance_accuracy_value', 'NONE');
#3111 = ORIENTED_EDGE ( 'NONE', *, *, #792, .F. ) ;
#3112 = DIRECTION ( 'NONE',  ( -1.752490724247359037E-17, 1.000000000000000000, 3.853078496550133260E-17 ) ) ;
#3113 = ORIENTED_EDGE ( 'NONE', *, *, #2452, .F. ) ;
#3114 = LINE ( 'NONE', #6361, #660 ) ;
#3115 = CARTESIAN_POINT ( 'NONE',  ( 0.000000000000000000, 0.000000000000000000, 20.00000000000000000 ) ) ;
#3116 = ORIENTED_EDGE ( 'NONE', *, *, #4151, .T. ) ;
#3117 = CIRCLE ( 'NONE', #7582, 8.000000000000000000 ) ;
#3118 = CARTESIAN_POINT ( 'NONE',  ( 11.86014387961076011, 48.57408496170469192, -16.53260109561406566 ) ) ;
#3119 = DIRECTION ( 'NONE',  ( 1.000000000000000000, 0.000000000000000000, 0.000000000000000000 ) ) ;
#3120 = VERTEX_POINT ( 'NONE', #4067 ) ;
#3121 = DIRECTION ( 'NONE',  ( -1.752490724247359037E-17, 1.000000000000000000, 3.853078496550133260E-17 ) ) ;
#3122 = EDGE_CURVE ( 'NONE', #4494, #3982, #839, .T. ) ;
#3123 = CARTESIAN_POINT ( 'NONE',  ( -10.84023063519268604, 48.81293515762427404, -18.77686690299335126 ) ) ;
#3124 = ORIENTED_EDGE ( 'NONE', *, *, #51, .T. ) ;
#3125 = VERTEX_POINT ( 'NONE', #6009 ) ;
#3126 = CARTESIAN_POINT ( 'NONE',  ( 1.530808498934191521E-15, 125.0000000000000000, 0.000000000000000000 ) ) ;
#3127 = AXIS2_PLACEMENT_3D ( 'NONE', #7811, #2648, #3263 ) ;
#3128 = ADVANCED_FACE ( 'NONE', ( #103 ), #7378, .F. ) ;
#3129 = CARTESIAN_POINT ( 'NONE',  ( 0.000000000000000000, 72.50000000000000000, -212.5000000000000568 ) ) ;
#3130 = EDGE_LOOP ( 'NONE', ( #6272, #6468, #8071, #5191 ) ) ;
#3131 = CARTESIAN_POINT ( 'NONE',  ( -10.61457161467472865, -48.86086578770956379, -19.11406644883055961 ) ) ;
#3132 = CARTESIAN_POINT ( 'NONE',  ( -9.554908546685398122E-15, 88.75000000000002842, -94.50000000000011369 ) ) ;
#3133 = EDGE_CURVE ( 'NONE', #1787, #1402, #1056, .T. ) ;
#3134 = EDGE_CURVE ( 'NONE', #4302, #5610, #2086, .T. ) ;
#3135 = EDGE_CURVE ( 'NONE', #5343, #8276, #787, .T. ) ;
#3136 = VECTOR ( 'NONE', #2946, 1000.000000000000000 ) ;
#3137 = AXIS2_PLACEMENT_3D ( 'NONE', #1327, #3896, #6466 ) ;
#3138 = CARTESIAN_POINT ( 'NONE',  ( 125.0000000000000000, -125.0000000000000000, 0.000000000000000000 ) ) ;
#3139 = CARTESIAN_POINT ( 'NONE',  ( 102.5000000000000000, 1.347111479062085446E-15, -9.499999999999952038 ) ) ;
#3140 = CYLINDRICAL_SURFACE ( 'NONE', #1704, 12.49999999999999289 ) ;
#3141 = CARTESIAN_POINT ( 'NONE',  ( 0.000000000000000000, 125.0000000000000568, 79.99999999999992895 ) ) ;
#3142 = CARTESIAN_POINT ( 'NONE',  ( 11.83759003446072455, 48.57866412327430794, -8.463974912767849190 ) ) ;
#3143 = FACE_BOUND ( 'NONE', #7490, .T. ) ;
#3144 = ORIENTED_EDGE ( 'NONE', *, *, #7161, .T. ) ;
#3145 = CIRCLE ( 'NONE', #3531, 37.50000000000000000 ) ;
#3146 = VERTEX_POINT ( 'NONE', #3465 ) ;
#3147 = ORIENTED_EDGE ( 'NONE', *, *, #3367, .F. ) ;
#3148 = CARTESIAN_POINT ( 'NONE',  ( -99.49999999999998579, 0.000000000000000000, 0.000000000000000000 ) ) ;
#3149 = EDGE_LOOP ( 'NONE', ( #2844, #4219 ) ) ;
#3150 = CARTESIAN_POINT ( 'NONE',  ( 99.99999999999991473, -115.0000000000000000, 250.0000000000000000 ) ) ;
#3151 = LINE ( 'NONE', #3748, #1433 ) ;
#3152 = VECTOR ( 'NONE', #4540, 1000.000000000000000 ) ;
#3153 = ITEM_DEFINED_TRANSFORMATION ( 'NONE', 'NONE', #6234,  #1299 ) ;
#3154 = EDGE_CURVE ( 'NONE', #3210, #1562, #6658, .T. ) ;
#3155 = ORIENTED_EDGE ( 'NONE', *, *, #3045, .F. ) ;
#3156 = DIRECTION ( 'NONE',  ( -0.000000000000000000, 1.266875999117951024E-16, 1.000000000000000000 ) ) ;
#3157 = ORIENTED_EDGE ( 'NONE', *, *, #3184, .F. ) ;
#3158 = AXIS2_PLACEMENT_3D ( 'NONE', #3340, #1943, #2608 ) ;
#3159 = DIRECTION ( 'NONE',  ( 0.000000000000000000, 0.000000000000000000, 1.000000000000000000 ) ) ;
#3160 = EDGE_LOOP ( 'NONE', ( #5157, #3998, #628, #7007, #3029, #2475 ) ) ;
#3161 = CARTESIAN_POINT ( 'NONE',  ( 14.30908802125418511, 4.500000000000000000, -126.0000000000000284 ) ) ;
#3162 = CARTESIAN_POINT ( 'NONE',  ( 114.9999999999999147, -115.0000000000000000, 250.0000000000000000 ) ) ;
#3163 = ORIENTED_EDGE ( 'NONE', *, *, #1711, .F. ) ;
#3164 = CARTESIAN_POINT ( 'NONE',  ( -1.236408833568031405E-20, 49.99999999999999289, -25.00000000000000000 ) ) ;
#3165 = DIRECTION ( 'NONE',  ( -0.000000000000000000, -7.945337353457666666E-18, -1.000000000000000000 ) ) ;
#3166 = CYLINDRICAL_SURFACE ( 'NONE', #7316, 12.99999999999999822 ) ;
#3167 = CARTESIAN_POINT ( 'NONE',  ( 0.000000000000000000, 0.000000000000000000, 15.00000000000000000 ) ) ;
#3168 = ORIENTED_EDGE ( 'NONE', *, *, #1780, .T. ) ;
#3169 = ORIENTED_EDGE ( 'NONE', *, *, #8157, .F. ) ;
#3170 = PRODUCT_RELATED_PRODUCT_CATEGORY ( 'part', '', ( #5056 ) ) ;
#3171 = CIRCLE ( 'NONE', #7910, 5.999999999999984901 ) ;
#3172 = CARTESIAN_POINT ( 'NONE',  ( 1.592040838891560279E-15, -72.49999999999998579, 92.99999999999995737 ) ) ;
#3173 = CONICAL_SURFACE ( 'NONE', #7653, 9.500000000000008882, 0.7853981633974466137 ) ;
#3174 = EDGE_CURVE ( 'NONE', #7809, #1626, #2731, .T. ) ;
#3175 = ADVANCED_FACE ( 'NONE', ( #5273 ), #231, .F. ) ;
#3176 = DIRECTION ( 'NONE',  ( 0.000000000000000000, -1.000000000000000000, 1.266875999117951024E-16 ) ) ;
#3177 = CARTESIAN_POINT ( 'NONE',  ( 10.16604137791875573, -48.95616179457642403, -5.215114234092022905 ) ) ;
#3178 = LINE ( 'NONE', #3107, #7784 ) ;
#3179 = FACE_OUTER_BOUND ( 'NONE', #4817, .T. ) ;
#3180 = EDGE_LOOP ( 'NONE', ( #336, #972, #1810, #2891 ) ) ;
#3181 = FACE_OUTER_BOUND ( 'NONE', #2968, .T. ) ;
#3182 = CONICAL_SURFACE ( 'NONE', #1854, 5.999999999999991118, 1.029744258676652313 ) ;
#3183 = VERTEX_POINT ( 'NONE', #2806 ) ;
#3184 = EDGE_CURVE ( 'NONE', #7934, #6392, #3386, .T. ) ;
#3185 = UNCERTAINTY_MEASURE_WITH_UNIT (LENGTH_MEASURE( 1.000000000000000082E-05 ), #1380, 'distance_accuracy_value', 'NONE');
#3186 = EDGE_LOOP ( 'NONE', ( #3088, #6469, #3532, #4873 ) ) ;
#3187 = EDGE_CURVE ( 'NONE', #1109, #1665, #184, .T. ) ;
#3188 = CARTESIAN_POINT ( 'NONE',  ( 60.00000000000000000, -55.00000000000000000, 240.0000000000000284 ) ) ;
#3189 = EDGE_CURVE ( 'NONE', #4072, #3924, #3988, .T. ) ;
#3190 = EDGE_LOOP ( 'NONE', ( #7937, #1108 ) ) ;
#3191 = DIRECTION ( 'NONE',  ( 0.000000000000000000, -1.000000000000000000, 9.256405414277014607E-16 ) ) ;
#3192 = CARTESIAN_POINT ( 'NONE',  ( -120.0000000000000000, -125.0000000000000000, -28.00000000000002487 ) ) ;
#3193 = AXIS2_PLACEMENT_3D ( 'NONE', #1288, #3856, #2834 ) ;
#3194 = CARTESIAN_POINT ( 'NONE',  ( 11.21042436406066578, 48.72746226073035558, -18.04468079945885250 ) ) ;
#3195 = AXIS2_PLACEMENT_3D ( 'NONE', #7885, #2610, #3261 ) ;
#3196 = ORIENTED_EDGE ( 'NONE', *, *, #6952, .T. ) ;
#3197 = PLANE ( 'NONE',  #47 ) ;
#3198 = ADVANCED_FACE ( 'NONE', ( #798, #2248 ), #2763, .F. ) ;
#3199 = CARTESIAN_POINT ( 'NONE',  ( 0.000000000000000000, 2.635170283421476540E-17, -246.6833752096445664 ) ) ;
#3200 = VECTOR ( 'NONE', #1017, 1000.000000000000000 ) ;
#3201 = ORIENTED_EDGE ( 'NONE', *, *, #6275, .F. ) ;
#3202 = CARTESIAN_POINT ( 'NONE',  ( 125.0000000000000000, -125.0000000000000568, -9.184850993605156622E-15 ) ) ;
#3203 = VECTOR ( 'NONE', #4288, 1000.000000000000000 ) ;
#3204 = CARTESIAN_POINT ( 'NONE',  ( -121.0000000000000284, -115.0000000000000000, 20.00000000000000355 ) ) ;
#3205 = CARTESIAN_POINT ( 'NONE',  ( -8.258796090566862702, 49.31668406204208566, -21.91840799305900589 ) ) ;
#3206 = ORIENTED_EDGE ( 'NONE', *, *, #3954, .T. ) ;
#3207 = LINE ( 'NONE', #564, #2794 ) ;
#3208 = VECTOR ( 'NONE', #5178, 1000.000000000000000 ) ;
#3209 = DIRECTION ( 'NONE',  ( -1.000000000000000000, -0.000000000000000000, -0.000000000000000000 ) ) ;
#3210 = VERTEX_POINT ( 'NONE', #3306 ) ;
#3211 = CARTESIAN_POINT ( 'NONE',  ( -109.0000000000000426, -115.0000000000000000, 20.00000000000000355 ) ) ;
#3212 = APPLICATION_CONTEXT ( 'automotive_design' ) ;
#3213 = VERTEX_POINT ( 'NONE', #4749 ) ;
#3214 = VECTOR ( 'NONE', #3821, 1000.000000000000000 ) ;
#3215 = AXIS2_PLACEMENT_3D ( 'NONE', #3104, #2397, #5681 ) ;
#3216 = LINE ( 'NONE', #7674, #6696 ) ;
#3217 = LINE ( 'NONE', #4351, #3214 ) ;
#3218 = CARTESIAN_POINT ( 'NONE',  ( 12.41973075191816811, -48.43322590808266170, -10.86594944112157535 ) ) ;
#3219 = AXIS2_PLACEMENT_3D ( 'NONE', #300, #7958, #7320 ) ;
#3220 = DIRECTION ( 'NONE',  ( -0.000000000000000000, -0.000000000000000000, 1.000000000000000000 ) ) ;
#3221 = VECTOR ( 'NONE', #5579, 1000.000000000000000 ) ;
#3222 = DIRECTION ( 'NONE',  ( -1.000000000000000000, -0.000000000000000000, 0.000000000000000000 ) ) ;
#3223 = EDGE_CURVE ( 'NONE', #5090, #57, #1515, .T. ) ;
#3224 = ORIENTED_EDGE ( 'NONE', *, *, #1745, .T. ) ;
#3225 = CIRCLE ( 'NONE', #5264, 8.000000000000000000 ) ;
#3226 = ORIENTED_EDGE ( 'NONE', *, *, #335, .T. ) ;
#3227 = EDGE_LOOP ( 'NONE', ( #3384, #5341, #508, #6780 ) ) ;
#3228 = CYLINDRICAL_SURFACE ( 'NONE', #5653, 5.999999999999991118 ) ;
#3229 = ORIENTED_EDGE ( 'NONE', *, *, #1359, .F. ) ;
#3230 = DIRECTION ( 'NONE',  ( 1.000000000000000000, 0.000000000000000000, 0.000000000000000000 ) ) ;
#3231 = CARTESIAN_POINT ( 'NONE',  ( 108.9999999999999147, 115.0000000000000000, 0.000000000000000000 ) ) ;
#3232 = ADVANCED_FACE ( 'NONE', ( #4106 ), #2023, .F. ) ;
#3233 = DIRECTION ( 'NONE',  ( 1.000000000000000000, 0.000000000000000000, 0.000000000000000000 ) ) ;
#3234 = DIRECTION ( 'NONE',  ( 1.000000000000000000, 0.000000000000000000, 0.000000000000000000 ) ) ;
#3235 = ADVANCED_FACE ( 'NONE', ( #270 ), #7391, .F. ) ;
#3236 = EDGE_CURVE ( 'NONE', #4851, #8231, #2121, .T. ) ;
#3237 = EDGE_CURVE ( 'NONE', #6772, #8146, #4030, .T. ) ;
#3238 = EDGE_LOOP ( 'NONE', ( #3403, #5267, #6886, #7093 ) ) ;
#3239 = CARTESIAN_POINT ( 'NONE',  ( 17.61817604250836311, -4.500000000000000000, -126.0000000000000284 ) ) ;
#3240 = CARTESIAN_POINT ( 'NONE',  ( 55.00000000000000000, -55.00000000000000000, 240.0000000000000284 ) ) ;
#3241 = ORIENTED_EDGE ( 'NONE', *, *, #6708, .F. ) ;
#3242 = ORIENTED_EDGE ( 'NONE', *, *, #5058, .T. ) ;
#3243 = CARTESIAN_POINT ( 'NONE',  ( -12.17681684015966681, 48.49465898589869539, -15.35333092327343429 ) ) ;
#3244 = CARTESIAN_POINT ( 'NONE',  ( 0.000000000000000000, 125.0000000000000000, -12.50000000000000000 ) ) ;
#3245 = CIRCLE ( 'NONE', #5948, 5.999999999999991118 ) ;
#3246 = DIRECTION ( 'NONE',  ( 1.000000000000000000, 0.000000000000000000, -0.000000000000000000 ) ) ;
#3247 = CARTESIAN_POINT ( 'NONE',  ( -59.99999999999999289, -55.00000000000000000, 220.0000000000000284 ) ) ;
#3248 = DIRECTION ( 'NONE',  ( 0.8571673007021134438, 0.000000000000000000, 0.5150380749100522682 ) ) ;
#3249 = CYLINDRICAL_SURFACE ( 'NONE', #3777, 12.50000000000000000 ) ;
#3250 = VERTEX_POINT ( 'NONE', #1718 ) ;
#3251 = LINE ( 'NONE', #5916, #7651 ) ;
#3252 = CARTESIAN_POINT ( 'NONE',  ( 0.000000000000000000, 0.000000000000000000, 98.00000000000002842 ) ) ;
#3253 = EDGE_CURVE ( 'NONE', #8231, #2791, #6577, .T. ) ;
#3254 = ORIENTED_EDGE ( 'NONE', *, *, #991, .F. ) ;
#3255 = VECTOR ( 'NONE', #503, 1000.000000000000000 ) ;
#3256 = DIRECTION ( 'NONE',  ( -0.000000000000000000, -0.000000000000000000, 1.000000000000000000 ) ) ;
#3257 = CARTESIAN_POINT ( 'NONE',  ( -95.00000000000000000, 95.00000000000008527, 35.00000000000000000 ) ) ;
#3258 = CARTESIAN_POINT ( 'NONE',  ( 12.50025679328619788, -48.41222552385477940, -11.67941733774923030 ) ) ;
#3259 = DIRECTION ( 'NONE',  ( -0.000000000000000000, -0.000000000000000000, 1.000000000000000000 ) ) ;
#3260 = PRODUCT_DEFINITION_FORMATION_WITH_SPECIFIED_SOURCE ( 'ANY', '', #7894, .NOT_KNOWN. ) ;
#3261 = DIRECTION ( 'NONE',  ( 0.000000000000000000, 0.000000000000000000, -1.000000000000000000 ) ) ;
#3262 = ORIENTED_EDGE ( 'NONE', *, *, #4902, .T. ) ;
#3263 = DIRECTION ( 'NONE',  ( 0.000000000000000000, 0.000000000000000000, -1.000000000000000000 ) ) ;
#3264 = ORIENTED_EDGE ( 'NONE', *, *, #937, .F. ) ;
#3265 = ORIENTED_EDGE ( 'NONE', *, *, #3764, .T. ) ;
#3266 = DIRECTION ( 'NONE',  ( 0.000000000000000000, 0.000000000000000000, -1.000000000000000000 ) ) ;
#3267 = VERTEX_POINT ( 'NONE', #6132 ) ;
#3268 = DIRECTION ( 'NONE',  ( 1.000000000000000000, 0.000000000000000000, 0.000000000000000000 ) ) ;
#3269 = DIRECTION ( 'NONE',  ( -0.000000000000000000, -7.945337353457666666E-18, -1.000000000000000000 ) ) ;
#3270 = CONTEXT_DEPENDENT_SHAPE_REPRESENTATION ( #7215, #1771 ) ;
#3271 = DIRECTION ( 'NONE',  ( -0.000000000000000000, -0.000000000000000000, 1.000000000000000000 ) ) ;
#3272 = VECTOR ( 'NONE', #172, 1000.000000000000000 ) ;
#3273 = ORIENTED_EDGE ( 'NONE', *, *, #2382, .T. ) ;
#3274 = LINE ( 'NONE', #5145, #1276 ) ;
#3275 = LINE ( 'NONE', #6536, #3329 ) ;
#3276 = ORIENTED_EDGE ( 'NONE', *, *, #1646, .F. ) ;
#3277 = EDGE_CURVE ( 'NONE', #7206, #3072, #6028, .T. ) ;
#3278 = ADVANCED_FACE ( 'NONE', ( #4911 ), #7548, .F. ) ;
#3279 = EDGE_CURVE ( 'NONE', #2665, #4302, #5472, .T. ) ;
#3280 = CARTESIAN_POINT ( 'NONE',  ( -49.00000000000000711, 55.00000000000000711, -27.50000000000000000 ) ) ;
#3281 = CARTESIAN_POINT ( 'NONE',  ( -7.296436711415922538, 49.46595054402523317, -2.342244756090384961 ) ) ;
#3282 = CARTESIAN_POINT ( 'NONE',  ( -102.5000000000000000, 0.000000000000000000, 12.50000000000000000 ) ) ;
#3283 = ORIENTED_EDGE ( 'NONE', *, *, #2184, .T. ) ;
#3284 = FACE_BOUND ( 'NONE', #5189, .T. ) ;
#3285 = CARTESIAN_POINT ( 'NONE',  ( -94.99999999999998579, -1.387778780781444098E-14, 35.00000000000000000 ) ) ;
#3286 = ADVANCED_FACE ( 'NONE', ( #5558 ), #7591, .F. ) ;
#3287 = DIRECTION ( 'NONE',  ( -1.000000000000000000, 0.000000000000000000, 0.000000000000000000 ) ) ;
#3288 = CARTESIAN_POINT ( 'NONE',  ( 1.000000000000000888, 0.000000000000000000, 0.000000000000000000 ) ) ;
#3289 = VERTEX_POINT ( 'NONE', #6774 ) ;
#3290 = DIRECTION ( 'NONE',  ( -0.000000000000000000, -0.000000000000000000, 1.000000000000000000 ) ) ;
#3291 = CARTESIAN_POINT ( 'NONE',  ( 55.00000000000002132, -54.99999999999998579, -56.59999999999999432 ) ) ;
#3292 = VERTEX_POINT ( 'NONE', #4829 ) ;
#3293 = MECHANICAL_DESIGN_GEOMETRIC_PRESENTATION_REPRESENTATION (  '', ( #7355 ), #4226 ) ;
#3294 = LINE ( 'NONE', #1255, #4527 ) ;
#3295 = ADVANCED_FACE ( 'NONE', ( #3553 ), #4311, .T. ) ;
#3296 = ADVANCED_FACE ( 'NONE', ( #2283 ), #4223, .F. ) ;
#3297 = DIRECTION ( 'NONE',  ( 0.000000000000000000, 0.000000000000000000, 1.000000000000000000 ) ) ;
#3298 =( NAMED_UNIT ( * ) PLANE_ANGLE_UNIT ( ) SI_UNIT ( $, .RADIAN. ) );
#3299 = EDGE_LOOP ( 'NONE', ( #7878, #8141 ) ) ;
#3300 = ORIENTED_EDGE ( 'NONE', *, *, #4940, .F. ) ;
#3301 = ORIENTED_EDGE ( 'NONE', *, *, #505, .T. ) ;
#3302 = DIRECTION ( 'NONE',  ( 0.000000000000000000, 0.000000000000000000, -1.000000000000000000 ) ) ;
#3303 = AXIS2_PLACEMENT_3D ( 'NONE', #736, #3290, #5959 ) ;
#3304 = ORIENTED_EDGE ( 'NONE', *, *, #5622, .F. ) ;
#3305 = DIRECTION ( 'NONE',  ( 0.000000000000000000, -0.5000000000000011102, -0.8660254037844379305 ) ) ;
#3306 = CARTESIAN_POINT ( 'NONE',  ( -125.0000000000000000, 125.0000000000000000, 340.0000000000000000 ) ) ;
#3307 = CONTEXT_DEPENDENT_SHAPE_REPRESENTATION ( #2069, #1233 ) ;
#3308 = DIRECTION ( 'NONE',  ( 1.000000000000000000, 0.000000000000000000, 0.000000000000000000 ) ) ;
#3309 = VERTEX_POINT ( 'NONE', #440 ) ;
#3310 = CARTESIAN_POINT ( 'NONE',  ( 115.0000000000000000, -114.9999999999999716, 20.00000000000000000 ) ) ;
#3311 = LINE ( 'NONE', #3700, #3405 ) ;
#3312 = ORIENTED_EDGE ( 'NONE', *, *, #505, .F. ) ;
#3313 =( REPRESENTATION_RELATIONSHIP ('NONE','NONE', #6882, #239 ) REPRESENTATION_RELATIONSHIP_WITH_TRANSFORMATION ( #6531 )SHAPE_REPRESENTATION_RELATIONSHIP( ) );
#3314 = DIRECTION ( 'NONE',  ( 0.000000000000000000, 0.000000000000000000, -1.000000000000000000 ) ) ;
#3315 = AXIS2_PLACEMENT_3D ( 'NONE', #3901, #8342, #5844 ) ;
#3316 = AXIS2_PLACEMENT_3D ( 'NONE', #2840, #7368, #5337 ) ;
#3317 = CARTESIAN_POINT ( 'NONE',  ( -4.044723210857149809, 49.83770199522208344, -0.6652966195906341307 ) ) ;
#3318 = ADVANCED_FACE ( 'NONE', ( #6183 ), #6687, .F. ) ;
#3319 = EDGE_CURVE ( 'NONE', #4648, #4314, #2927, .T. ) ;
#3320 = AXIS2_PLACEMENT_3D ( 'NONE', #1886, #2633, #6460 ) ;
#3321 = DIRECTION ( 'NONE',  ( 0.000000000000000000, 0.000000000000000000, 1.000000000000000000 ) ) ;
#3322 = CARTESIAN_POINT ( 'NONE',  ( -102.5000000000000000, 1.163414459189986668E-15, 9.500000000000008882 ) ) ;
#3323 = LINE ( 'NONE', #851, #7741 ) ;
#3324 = AXIS2_PLACEMENT_3D ( 'NONE', #7462, #5642, #965 ) ;
#3325 = CARTESIAN_POINT ( 'NONE',  ( 0.000000000000000000, 0.000000000000000000, 27.50000000000000000 ) ) ;
#3326 = CARTESIAN_POINT ( 'NONE',  ( -94.99999999999997158, -95.00000000000008527, 70.00000000000000000 ) ) ;
#3327 = ORIENTED_EDGE ( 'NONE', *, *, #7529, .F. ) ;
#3328 = LINE ( 'NONE', #7277, #4383 ) ;
#3329 = VECTOR ( 'NONE', #4636, 1000.000000000000000 ) ;
#3330 = ORIENTED_EDGE ( 'NONE', *, *, #7745, .T. ) ;
#3331 = EDGE_CURVE ( 'NONE', #5909, #4789, #8089, .T. ) ;
#3332 = EDGE_CURVE ( 'NONE', #3595, #4172, #765, .T. ) ;
#3333 = EDGE_CURVE ( 'NONE', #6102, #8341, #4871, .T. ) ;
#3334 = DIRECTION ( 'NONE',  ( 0.000000000000000000, 1.000000000000000000, 0.000000000000000000 ) ) ;
#3335 = VECTOR ( 'NONE', #5390, 1000.000000000000000 ) ;
#3336 = AXIS2_PLACEMENT_3D ( 'NONE', #6918, #493, #6481 ) ;
#3337 = DIRECTION ( 'NONE',  ( 0.000000000000000000, -0.000000000000000000, -1.000000000000000000 ) ) ;
#3338 = LINE ( 'NONE', #1458, #4026 ) ;
#3339 = CARTESIAN_POINT ( 'NONE',  ( 0.000000000000000000, 5.000000000000000000, 0.000000000000000000 ) ) ;
#3340 = CARTESIAN_POINT ( 'NONE',  ( 10.00000000000000000, 57.99999999999990052, 93.75000000000004263 ) ) ;
#3341 = CIRCLE ( 'NONE', #7947, 5.999999999999991118 ) ;
#3342 = AXIS2_PLACEMENT_3D ( 'NONE', #1151, #1739, #8110 ) ;
#3343 = DIRECTION ( 'NONE',  ( -0.000000000000000000, 0.000000000000000000, 1.000000000000000000 ) ) ;
#3344 = EDGE_LOOP ( 'NONE', ( #3062, #290, #4509, #1842 ) ) ;
#3345 = EDGE_CURVE ( 'NONE', #6862, #5826, #1849, .T. ) ;
#3346 = CYLINDRICAL_SURFACE ( 'NONE', #583, 5.999999999999991118 ) ;
#3347 = CARTESIAN_POINT ( 'NONE',  ( 0.000000000000000000, 1.986334338364416506E-15, 0.000000000000000000 ) ) ;
#3348 = CIRCLE ( 'NONE', #3904, 20.00000000000000355 ) ;
#3349 = AXIS2_PLACEMENT_3D ( 'NONE', #1653, #7485, #6205 ) ;
#3350 = VERTEX_POINT ( 'NONE', #6818 ) ;
#3351 = CARTESIAN_POINT ( 'NONE',  ( 10.00000000000000000, 57.99999999999990052, 93.75000000000004263 ) ) ;
#3352 = CARTESIAN_POINT ( 'NONE',  ( 115.0000000000000000, 114.9999999999999716, 20.00000000000000000 ) ) ;
#3353 = CARTESIAN_POINT ( 'NONE',  ( 125.0000000000000000, 52.49999999999997158, 0.000000000000000000 ) ) ;
#3354 = VECTOR ( 'NONE', #1493, 1000.000000000000114 ) ;
#3355 = CARTESIAN_POINT ( 'NONE',  ( 5.000000000000000000, 2.342598717236915373, 4.057499999999997442 ) ) ;
#3356 = ORIENTED_EDGE ( 'NONE', *, *, #7989, .T. ) ;
#3357 = AXIS2_PLACEMENT_3D ( 'NONE', #5488, #1732, #7514 ) ;
#3358 = CARTESIAN_POINT ( 'NONE',  ( 14.30908802125418511, 4.500000000000000000, -118.0000000000000284 ) ) ;
#3359 = FACE_OUTER_BOUND ( 'NONE', #5904, .T. ) ;
#3360 = APPLICATION_CONTEXT ( 'automotive_design' ) ;
#3361 = CARTESIAN_POINT ( 'NONE',  ( 109.5000000000000142, 114.9999999999999716, 10.00000000000000000 ) ) ;
#3362 = FACE_OUTER_BOUND ( 'NONE', #7700, .T. ) ;
#3363 = AXIS2_PLACEMENT_3D ( 'NONE', #6240, #8238, #5740 ) ;
#3364 = CARTESIAN_POINT ( 'NONE',  ( 125.0000000000000000, -52.49999999999997158, 0.000000000000000000 ) ) ;
#3365 = FACE_OUTER_BOUND ( 'NONE', #705, .T. ) ;
#3366 = CARTESIAN_POINT ( 'NONE',  ( 4.999999999999994671, 4.969004387540385421E-16, -4.057500000000000107 ) ) ;
#3367 = EDGE_CURVE ( 'NONE', #48, #986, #2830, .T. ) ;
#3368 = ORIENTED_EDGE ( 'NONE', *, *, #7209, .F. ) ;
#3369 = DIRECTION ( 'NONE',  ( 0.000000000000000000, 0.000000000000000000, -1.000000000000000000 ) ) ;
#3370 = CIRCLE ( 'NONE', #6486, 5.999999999999991118 ) ;
#3371 = FACE_OUTER_BOUND ( 'NONE', #2856, .T. ) ;
#3372 = ADVANCED_FACE ( 'NONE', ( #6988 ), #3140, .F. ) ;
#3373 = CARTESIAN_POINT ( 'NONE',  ( 0.000000000000000000, 0.000000000000000000, 0.000000000000000000 ) ) ;
#3374 = DIRECTION ( 'NONE',  ( -0.000000000000000000, -0.000000000000000000, 1.000000000000000000 ) ) ;
#3375 = EDGE_CURVE ( 'NONE', #5439, #5603, #2904, .T. ) ;
#3376 = EDGE_CURVE ( 'NONE', #6775, #3808, #1257, .T. ) ;
#3377 = DIRECTION ( 'NONE',  ( -0.000000000000000000, -0.000000000000000000, -1.000000000000000000 ) ) ;
#3378 = ADVANCED_FACE ( 'NONE', ( #3822 ), #3173, .T. ) ;
#3379 =( NAMED_UNIT ( * ) SI_UNIT ( $, .STERADIAN. ) SOLID_ANGLE_UNIT ( ) );
#3380 = AXIS2_PLACEMENT_3D ( 'NONE', #2877, #1549, #6614 ) ;
#3381 = ORIENTED_EDGE ( 'NONE', *, *, #7081, .T. ) ;
#3382 = DIRECTION ( 'NONE',  ( -0.000000000000000000, -0.000000000000000000, 1.000000000000000000 ) ) ;
#3383 = CARTESIAN_POINT ( 'NONE',  ( 0.000000000000000000, 0.000000000000000000, -248.3416876048222832 ) ) ;
#3384 = ORIENTED_EDGE ( 'NONE', *, *, #131, .T. ) ;
#3385 = CARTESIAN_POINT ( 'NONE',  ( 0.000000000000000000, 125.0000000000000000, -12.50000000000000000 ) ) ;
#3386 = LINE ( 'NONE', #7297, #4260 ) ;
#3387 =( GEOMETRIC_REPRESENTATION_CONTEXT ( 3 ) GLOBAL_UNCERTAINTY_ASSIGNED_CONTEXT ( ( #2454 ) ) GLOBAL_UNIT_ASSIGNED_CONTEXT ( ( #5550, #1078, #4945 ) ) REPRESENTATION_CONTEXT ( 'NONE', 'WORKASPACE' ) );
#3388 = FACE_OUTER_BOUND ( 'NONE', #3458, .T. ) ;
#3389 = LINE ( 'NONE', #7859, #1107 ) ;
#3390 = ORIENTED_EDGE ( 'NONE', *, *, #1185, .T. ) ;
#3391 = DIRECTION ( 'NONE',  ( -0.000000000000000000, -0.000000000000000000, 1.000000000000000000 ) ) ;
#3392 = ORIENTED_EDGE ( 'NONE', *, *, #6689, .T. ) ;
#3393 = DIRECTION ( 'NONE',  ( -1.000000000000000000, -0.000000000000000000, -0.000000000000000000 ) ) ;
#3394 = EDGE_CURVE ( 'NONE', #5338, #6480, #7645, .T. ) ;
#3395 = VECTOR ( 'NONE', #2862, 1000.000000000000000 ) ;
#3396 = CARTESIAN_POINT ( 'NONE',  ( -125.0000000000000000, 120.0000000000000000, 0.000000000000000000 ) ) ;
#3397 = CARTESIAN_POINT ( 'NONE',  ( 125.0000000000000000, -125.0000000000000568, -9.184850993605156622E-15 ) ) ;
#3398 = CARTESIAN_POINT ( 'NONE',  ( 0.000000000000000000, 125.0000000000000000, -25.00000000000000000 ) ) ;
#3399 = CARTESIAN_POINT ( 'NONE',  ( 99.99999999999991473, -115.0000000000000000, 0.000000000000000000 ) ) ;
#3400 = CARTESIAN_POINT ( 'NONE',  ( 55.00000000000000711, 75.00000000000000000, 27.50000000000000000 ) ) ;
#3401 = DIRECTION ( 'NONE',  ( 1.000000000000000000, 0.000000000000000000, 0.000000000000000000 ) ) ;
#3402 = CARTESIAN_POINT ( 'NONE',  ( -109.0000000000000142, 115.0000000000000000, 70.00000000000000000 ) ) ;
#3403 = ORIENTED_EDGE ( 'NONE', *, *, #1780, .F. ) ;
#3404 = CARTESIAN_POINT ( 'NONE',  ( -109.4999999999999858, 114.9999999999999858, 10.00000000000000000 ) ) ;
#3405 = VECTOR ( 'NONE', #4363, 1000.000000000000000 ) ;
#3406 = VERTEX_POINT ( 'NONE', #1379 ) ;
#3407 = CARTESIAN_POINT ( 'NONE',  ( 80.00000000000000000, 5.616230220889804839E-16, -4.171999999999999709 ) ) ;
#3408 = B_SPLINE_CURVE_WITH_KNOTS ( 'NONE', 3,
 ( #3164, #4502, #5110, #3842, #7095, #4423, #4378, #1879, #7707, #4466, #3205, #1923, #7053, #1835, #6407, #3123, #8248, #1274, #2506, #5154, #3243, #7614, #6457, #5705, #8201, #7017, #1154, #1198, #3767, #3716, #6290, #3087, #5669, #558, #5066, #7659, #1240, #4546, #3281, #1524, #154, #7905, #3317, #5868, #5905, #4641, #114, #7939 ),
 .UNSPECIFIED., .F., .F.,
 ( 4, 2, 2, 2, 2, 2, 2, 2, 2, 2, 2, 2, 2, 2, 2, 2, 2, 2, 2, 2, 2, 2, 2, 4 ),
 ( 0.03923685324657887746, 0.04168849572278652410, 0.04414013819899417074, 0.04536595943709799406, 0.04659178067520181737, 0.04904342315140946401, 0.05026924438951328733, 0.05149506562761710371, 0.05394670810382474341, 0.05517252934192855979, 0.05639835058003238311, 0.05762417181813619949, 0.05884999305624001587, 0.06130163553244766250, 0.06375327800865530914, 0.06620492048486295578, 0.06743074172296677216, 0.06865656296107058854, 0.06988238419917441879, 0.07110820543727824905, 0.07355984791348588181, 0.07478566915158971207, 0.07601149038969352845, 0.07846313286590117508 ),
 .UNSPECIFIED. ) ;
#3409 = CIRCLE ( 'NONE', #3546, 15.00000000000000178 ) ;
#3410 = PRODUCT_DEFINITION_SHAPE ( 'NONE', 'NONE',  #4147 ) ;
#3411 = CARTESIAN_POINT ( 'NONE',  ( 124.9999999999997442, -125.0000000000000000, 20.00000000000000000 ) ) ;
#3412 = CARTESIAN_POINT ( 'NONE',  ( 50.00000000000000711, -55.00000000000000000, 220.0000000000000284 ) ) ;
#3413 = DIRECTION ( 'NONE',  ( 1.000000000000000000, 0.000000000000000000, 0.000000000000000000 ) ) ;
#3414 = CARTESIAN_POINT ( 'NONE',  ( 4.999999999999994671, 0.000000000000000000, 0.000000000000000000 ) ) ;
#3415 = EDGE_CURVE ( 'NONE', #7860, #2083, #2114, .T. ) ;
#3416 = LINE ( 'NONE', #217, #2273 ) ;
#3417 = ORIENTED_EDGE ( 'NONE', *, *, #190, .T. ) ;
#3418 = CARTESIAN_POINT ( 'NONE',  ( 120.0000000000000000, -120.0000000000000000, 0.000000000000000000 ) ) ;
#3419 = EDGE_CURVE ( 'NONE', #5233, #698, #3454, .T. ) ;
#3420 = ADVANCED_FACE ( 'NONE', ( #6044 ), #5998, .F. ) ;
#3421 = LINE ( 'NONE', #17, #3467 ) ;
#3422 = CYLINDRICAL_SURFACE ( 'NONE', #6936, 5.000000000000035527 ) ;
#3423 = ORIENTED_EDGE ( 'NONE', *, *, #7056, .F. ) ;
#3424 = CARTESIAN_POINT ( 'NONE',  ( -75.00000000000000000, -75.00000000000000000, -27.50000000000000000 ) ) ;
#3425 = DIRECTION ( 'NONE',  ( -0.000000000000000000, -0.000000000000000000, 1.000000000000000000 ) ) ;
#3426 = CARTESIAN_POINT ( 'NONE',  ( 0.000000000000000000, 0.000000000000000000, 20.00000000000000355 ) ) ;
#3427 = DIRECTION ( 'NONE',  ( 1.000000000000000000, 0.000000000000000000, 0.000000000000000000 ) ) ;
#3428 = EDGE_CURVE ( 'NONE', #5586, #4375, #6609, .T. ) ;
#3429 = ORIENTED_EDGE ( 'NONE', *, *, #3873, .T. ) ;
#3430 = EDGE_CURVE ( 'NONE', #5443, #7579, #2127, .T. ) ;
#3431 = AXIS2_PLACEMENT_3D ( 'NONE', #1218, #7805, #6389 ) ;
#3432 = EDGE_LOOP ( 'NONE', ( #2128, #7481, #1576, #778 ) ) ;
#3433 = LINE ( 'NONE', #6017, #7819 ) ;
#3434 = VECTOR ( 'NONE', #3413, 1000.000000000000000 ) ;
#3435 = ORIENTED_EDGE ( 'NONE', *, *, #5415, .T. ) ;
#3436 = DIRECTION ( 'NONE',  ( 1.000000000000000000, 0.000000000000000000, 0.000000000000000000 ) ) ;
#3437 = CARTESIAN_POINT ( 'NONE',  ( 0.000000000000000000, 105.0000000000000426, 79.99999999999992895 ) ) ;
#3438 = DIRECTION ( 'NONE',  ( 1.000000000000000000, 0.000000000000000000, 0.000000000000000000 ) ) ;
#3439 = EDGE_CURVE ( 'NONE', #1787, #4917, #744, .T. ) ;
#3440 = DIRECTION ( 'NONE',  ( -1.000000000000000000, -0.000000000000000000, -0.000000000000000000 ) ) ;
#3441 = CYLINDRICAL_SURFACE ( 'NONE', #918, 12.50000000000000000 ) ;
#3442 = MANIFOLD_SOLID_BREP ( 'Chamfer1', #5981 ) ;
#3443 = CARTESIAN_POINT ( 'NONE',  ( 0.000000000000000000, 125.0000000000000000, -25.00000000000000000 ) ) ;
#3444 = FACE_BOUND ( 'NONE', #2376, .T. ) ;
#3445 = DIRECTION ( 'NONE',  ( -0.000000000000000000, -0.000000000000000000, 1.000000000000000000 ) ) ;
#3446 = CARTESIAN_POINT ( 'NONE',  ( -54.99999999999999289, -75.00000000000000000, 27.50000000000000000 ) ) ;
#3447 = ORIENTED_EDGE ( 'NONE', *, *, #6227, .T. ) ;
#3448 = ORIENTED_EDGE ( 'NONE', *, *, #7106, .F. ) ;
#3449 = VECTOR ( 'NONE', #1381, 1000.000000000000000 ) ;
#3450 = DIRECTION ( 'NONE',  ( -0.000000000000000000, -0.000000000000000000, 1.000000000000000000 ) ) ;
#3451 = FACE_OUTER_BOUND ( 'NONE', #8292, .T. ) ;
#3452 = VECTOR ( 'NONE', #7869, 1000.000000000000000 ) ;
#3453 = CARTESIAN_POINT ( 'NONE',  ( 49.00000000000000711, 55.00000000000000711, -27.50000000000000000 ) ) ;
#3454 = LINE ( 'NONE', #3941, #3434 ) ;
#3455 = AXIS2_PLACEMENT_3D ( 'NONE', #7857, #5311, #8005 ) ;
#3456 = CARTESIAN_POINT ( 'NONE',  ( -95.00000000000001421, 0.000000000000000000, 0.000000000000000000 ) ) ;
#3457 = DIRECTION ( 'NONE',  ( -0.000000000000000000, -0.000000000000000000, 1.000000000000000000 ) ) ;
#3458 = EDGE_LOOP ( 'NONE', ( #2913, #2358, #3113, #89 ) ) ;
#3459 = AXIS2_PLACEMENT_3D ( 'NONE', #5399, #7175, #6019 ) ;
#3460 = AXIS2_PLACEMENT_3D ( 'NONE', #1521, #4075, #6663 ) ;
#3461 = CARTESIAN_POINT ( 'NONE',  ( 115.0000000000000000, 115.0000000000000000, 70.00000000000000000 ) ) ;
#3462 = CARTESIAN_POINT ( 'NONE',  ( -60.00000000000000000, -55.00000000000000000, 240.0000000000000284 ) ) ;
#3463 = EDGE_LOOP ( 'NONE', ( #463, #870, #1186, #5696 ) ) ;
#3464 = FACE_OUTER_BOUND ( 'NONE', #3951, .T. ) ;
#3465 = CARTESIAN_POINT ( 'NONE',  ( 120.0000000000000000, -125.0000000000000000, 0.000000000000000000 ) ) ;
#3466 = AXIS2_PLACEMENT_3D ( 'NONE', #673, #1226, #3230 ) ;
#3467 = VECTOR ( 'NONE', #2614, 1000.000000000000000 ) ;
#3468 = ADVANCED_FACE ( 'NONE', ( #2753, #7846 ), #4613, .F. ) ;
#3469 = DIRECTION ( 'NONE',  ( -0.000000000000000000, -7.945337353457666666E-18, -1.000000000000000000 ) ) ;
#3470 = DIRECTION ( 'NONE',  ( -0.000000000000000000, -0.000000000000000000, 1.000000000000000000 ) ) ;
#3471 =( REPRESENTATION_RELATIONSHIP ('NONE','NONE', #6882, #239 ) REPRESENTATION_RELATIONSHIP_WITH_TRANSFORMATION ( #7379 )SHAPE_REPRESENTATION_RELATIONSHIP( ) );
#3472 = ORIENTED_EDGE ( 'NONE', *, *, #6646, .T. ) ;
#3473 = CIRCLE ( 'NONE', #4830, 54.99999999999995026 ) ;
#3474 = AXIS2_PLACEMENT_3D ( 'NONE', #5597, #41, #1844 ) ;
#3475 = ORIENTED_EDGE ( 'NONE', *, *, #4100, .T. ) ;
#3476 = DIRECTION ( 'NONE',  ( 0.000000000000000000, -1.000000000000000000, 0.000000000000000000 ) ) ;
#3477 = EDGE_CURVE ( 'NONE', #8205, #5186, #7197, .T. ) ;
#3478 = VERTEX_POINT ( 'NONE', #136 ) ;
#3479 = DIRECTION ( 'NONE',  ( -0.000000000000000000, -0.000000000000000000, -1.000000000000000000 ) ) ;
#3480 = ADVANCED_FACE ( 'NONE', ( #4018, #4094 ), #4701, .F. ) ;
#3481 = CARTESIAN_POINT ( 'NONE',  ( -115.0000000000000000, -114.9999999999999147, 108.4000000000000341 ) ) ;
#3482 = EDGE_CURVE ( 'NONE', #1112, #4879, #7096, .T. ) ;
#3483 = DIRECTION ( 'NONE',  ( -0.000000000000000000, -0.000000000000000000, 1.000000000000000000 ) ) ;
#3484 = EDGE_CURVE ( 'NONE', #4695, #8274, #1544, .T. ) ;
#3485 = AXIS2_PLACEMENT_3D ( 'NONE', #430, #5712, #8334 ) ;
#3486 = MECHANICAL_DESIGN_GEOMETRIC_PRESENTATION_REPRESENTATION (  '', ( #7953 ), #1481 ) ;
#3487 = EDGE_LOOP ( 'NONE', ( #6187, #3448, #4579, #1038 ) ) ;
#3488 = DIRECTION ( 'NONE',  ( 1.000000000000000000, 0.000000000000000000, 0.000000000000000000 ) ) ;
#3489 = DIRECTION ( 'NONE',  ( -1.000000000000000000, -0.000000000000000000, -0.000000000000000000 ) ) ;
#3490 = DIRECTION ( 'NONE',  ( -1.000000000000000000, 0.000000000000000000, -0.000000000000000000 ) ) ;
#3491 = LINE ( 'NONE', #2742, #5923 ) ;
#3492 = ORIENTED_EDGE ( 'NONE', *, *, #4092, .F. ) ;
#3493 = ORIENTED_EDGE ( 'NONE', *, *, #3639, .T. ) ;
#3494 = CARTESIAN_POINT ( 'NONE',  ( 55.00000000000000711, 54.99999999999999289, 27.50000000000000000 ) ) ;
#3495 = LINE ( 'NONE', #904, #3272 ) ;
#3496 = CARTESIAN_POINT ( 'NONE',  ( 0.000000000000000000, 0.000000000000000000, 35.00000000000000000 ) ) ;
#3497 = ADVANCED_FACE ( 'NONE', ( #7412 ), #6852, .F. ) ;
#3498 = VECTOR ( 'NONE', #5612, 1000.000000000000000 ) ;
#3499 =( NAMED_UNIT ( * ) SI_UNIT ( $, .STERADIAN. ) SOLID_ANGLE_UNIT ( ) );
#3500 = DIRECTION ( 'NONE',  ( -0.000000000000000000, -0.000000000000000000, 1.000000000000000000 ) ) ;
#3501 = CARTESIAN_POINT ( 'NONE',  ( 4.999999999999994671, 0.000000000000000000, 0.000000000000000000 ) ) ;
#3502 = ORIENTED_EDGE ( 'NONE', *, *, #2640, .T. ) ;
#3503 = DIRECTION ( 'NONE',  ( -0.000000000000000000, -0.000000000000000000, 1.000000000000000000 ) ) ;
#3504 = CARTESIAN_POINT ( 'NONE',  ( -120.0000000000000000, -115.0000000000000000, 270.0000000000000000 ) ) ;
#3505 = CARTESIAN_POINT ( 'NONE',  ( -115.0000000000000284, -115.0000000000000000, 70.00000000000000000 ) ) ;
#3506 = ORIENTED_EDGE ( 'NONE', *, *, #189, .F. ) ;
#3507 = CYLINDRICAL_SURFACE ( 'NONE', #7407, 4.999999999999997335 ) ;
#3508 = CARTESIAN_POINT ( 'NONE',  ( 10.40000000000000036, 0.000000000000000000, 0.000000000000000000 ) ) ;
#3509 = ITEM_DEFINED_TRANSFORMATION ( 'NONE', 'NONE', #6370,  #1299 ) ;
#3510 = DIRECTION ( 'NONE',  ( -0.000000000000000000, -1.000000000000000000, -0.000000000000000000 ) ) ;
#3511 = FACE_OUTER_BOUND ( 'NONE', #5551, .T. ) ;
#3512 = MANIFOLD_SOLID_BREP ( '\X2\00d8\X0\12.0mm Dowel Hole1', #1667 ) ;
#3513 = AXIS2_PLACEMENT_3D ( 'NONE', #5385, #3503, #7964 ) ;
#3514 = ORIENTED_EDGE ( 'NONE', *, *, #2278, .F. ) ;
#3515 = CARTESIAN_POINT ( 'NONE',  ( 105.0000000000000000, 105.0000000000000853, 20.00000000000000355 ) ) ;
#3516 = ORIENTED_EDGE ( 'NONE', *, *, #7217, .T. ) ;
#3517 = DIRECTION ( 'NONE',  ( 0.000000000000000000, -0.000000000000000000, -1.000000000000000000 ) ) ;
#3518 = DIRECTION ( 'NONE',  ( -6.591949208711848223E-16, 2.795409351640305996E-31, 0.9999999999999997780 ) ) ;
#3519 = ORIENTED_EDGE ( 'NONE', *, *, #3428, .F. ) ;
#3520 = CARTESIAN_POINT ( 'NONE',  ( 10.61691938675656566, 48.86036797030515544, -5.889423163904315750 ) ) ;
#3521 = CIRCLE ( 'NONE', #3817, 5.499999999999991118 ) ;
#3522 = PRODUCT_DEFINITION ( 'UNKNOWN', '', #2479, #6140 ) ;
#3523 = DIRECTION ( 'NONE',  ( 1.000000000000000000, 0.000000000000000000, 0.000000000000000000 ) ) ;
#3524 = PRODUCT_DEFINITION_FORMATION_WITH_SPECIFIED_SOURCE ( 'ANY', '', #5324, .NOT_KNOWN. ) ;
#3525 = EDGE_CURVE ( 'NONE', #2041, #5090, #2271, .T. ) ;
#3526 = DIRECTION ( 'NONE',  ( -0.000000000000000000, -0.000000000000000000, 1.000000000000000000 ) ) ;
#3527 = CARTESIAN_POINT ( 'NONE',  ( 17.61817604250836311, 4.500000000000000000, -118.0000000000000284 ) ) ;
#3528 = PLANE ( 'NONE',  #7058 ) ;
#3529 = CARTESIAN_POINT ( 'NONE',  ( -115.0000000000000142, -115.0000000000000000, 266.9956969048622568 ) ) ;
#3530 = VERTEX_POINT ( 'NONE', #4818 ) ;
#3531 = AXIS2_PLACEMENT_3D ( 'NONE', #4684, #7397, #4725 ) ;
#3532 = ORIENTED_EDGE ( 'NONE', *, *, #2345, .F. ) ;
#3533 = EDGE_CURVE ( 'NONE', #5749, #4086, #1173, .T. ) ;
#3534 = FACE_OUTER_BOUND ( 'NONE', #2045, .T. ) ;
#3535 = FACE_OUTER_BOUND ( 'NONE', #4398, .T. ) ;
#3536 = PLANE ( 'NONE',  #1480 ) ;
#3537 = CIRCLE ( 'NONE', #5175, 5.999999999999991118 ) ;
#3538 = ORIENTED_EDGE ( 'NONE', *, *, #8207, .T. ) ;
#3539 = CARTESIAN_POINT ( 'NONE',  ( -10.61691938675656921, -48.86036797030517675, -5.889423163904312197 ) ) ;
#3540 =( LENGTH_UNIT ( ) NAMED_UNIT ( * ) SI_UNIT ( .MILLI., .METRE. ) );
#3541 = DIRECTION ( 'NONE',  ( 0.000000000000000000, 0.000000000000000000, 1.000000000000000000 ) ) ;
#3542 = DIRECTION ( 'NONE',  ( -0.000000000000000000, -0.000000000000000000, 1.000000000000000000 ) ) ;
#3543 = VERTEX_POINT ( 'NONE', #432 ) ;
#3544 = FACE_OUTER_BOUND ( 'NONE', #2400, .T. ) ;
#3545 = CIRCLE ( 'NONE', #5725, 4.999999999999990230 ) ;
#3546 = AXIS2_PLACEMENT_3D ( 'NONE', #3373, #6725, #5581 ) ;
#3547 = EDGE_CURVE ( 'NONE', #986, #48, #4231, .T. ) ;
#3548 = LINE ( 'NONE', #6127, #2908 ) ;
#3549 = EDGE_CURVE ( 'NONE', #5775, #3690, #5802, .T. ) ;
#3550 = PLANE ( 'NONE',  #7826 ) ;
#3551 = EDGE_LOOP ( 'NONE', ( #6996, #6319, #1710 ) ) ;
#3552 = CARTESIAN_POINT ( 'NONE',  ( 0.000000000000000000, 0.000000000000000000, 20.00000000000000355 ) ) ;
#3553 = FACE_OUTER_BOUND ( 'NONE', #7625, .T. ) ;
#3554 = ORIENTED_EDGE ( 'NONE', *, *, #792, .T. ) ;
#3555 = DIRECTION ( 'NONE',  ( 0.000000000000000000, -1.000000000000000000, -2.960594732333750117E-16 ) ) ;
#3556 = CARTESIAN_POINT ( 'NONE',  ( -114.9999999999999858, -114.9999999999999858, 10.00000000000000000 ) ) ;
#3557 = ORIENTED_EDGE ( 'NONE', *, *, #5585, .F. ) ;
#3558 = CARTESIAN_POINT ( 'NONE',  ( 99.49999999999998579, 0.000000000000000000, 0.000000000000000000 ) ) ;
#3559 = ORIENTED_EDGE ( 'NONE', *, *, #1866, .T. ) ;
#3560 = CARTESIAN_POINT ( 'NONE',  ( -114.9999999999999716, 114.9999999999999858, 10.00000000000000000 ) ) ;
#3561 = DIRECTION ( 'NONE',  ( 1.000000000000000000, 0.000000000000000000, 0.000000000000000000 ) ) ;
#3562 = ORIENTED_EDGE ( 'NONE', *, *, #5168, .F. ) ;
#3563 = CARTESIAN_POINT ( 'NONE',  ( 60.99999999999998579, 55.00000000000000711, 27.50000000000000000 ) ) ;
#3564 = CIRCLE ( 'NONE', #8178, 9.000000000000007105 ) ;
#3565 = VECTOR ( 'NONE', #2360, 1000.000000000000000 ) ;
#3566 = FACE_OUTER_BOUND ( 'NONE', #478, .T. ) ;
#3567 = ORIENTED_EDGE ( 'NONE', *, *, #3333, .F. ) ;
#3568 = CARTESIAN_POINT ( 'NONE',  ( 114.9999999999999858, 115.0000000000000000, 266.9956969048622568 ) ) ;
#3569 = CONICAL_SURFACE ( 'NONE', #3303, 4.999999999999990230, 1.029744258676653201 ) ;
#3570 = EDGE_LOOP ( 'NONE', ( #481, #2833, #1003 ) ) ;
#3571 = ORIENTED_EDGE ( 'NONE', *, *, #4825, .F. ) ;
#3572 = EDGE_CURVE ( 'NONE', #7416, #1211, #4790, .T. ) ;
#3573 = DIRECTION ( 'NONE',  ( 1.000000000000000000, 0.000000000000000000, 0.000000000000000000 ) ) ;
#3574 = ADVANCED_FACE ( 'NONE', ( #7670, #3850 ), #5715, .F. ) ;
#3575 = ORIENTED_EDGE ( 'NONE', *, *, #1907, .F. ) ;
#3576 = CARTESIAN_POINT ( 'NONE',  ( 0.000000000000000000, -49.99999999999999289, 0.000000000000000000 ) ) ;
#3577 = ORIENTED_EDGE ( 'NONE', *, *, #5620, .F. ) ;
#3578 = AXIS2_PLACEMENT_3D ( 'NONE', #4517, #3256, #5167 ) ;
#3579 = DIRECTION ( 'NONE',  ( -1.000000000000000000, -0.000000000000000000, 0.000000000000000000 ) ) ;
#3580 = CARTESIAN_POINT ( 'NONE',  ( 120.9999999999999005, -115.0000000000000000, 8.205133554287239938E-16 ) ) ;
#3581 = EDGE_LOOP ( 'NONE', ( #3633, #301, #5971, #5429 ) ) ;
#3582 = CARTESIAN_POINT ( 'NONE',  ( -9.415432556623350990, -49.10895683582203475, -4.238112224658973304 ) ) ;
#3583 = MANIFOLD_SOLID_BREP ( 'Boss-Extrude1', #6653 ) ;
#3584 = CIRCLE ( 'NONE', #507, 95.00000000000001421 ) ;
#3585 = EDGE_CURVE ( 'NONE', #4085, #5646, #7504, .T. ) ;
#3586 = ADVANCED_FACE ( 'NONE', ( #1326 ), #7232, .F. ) ;
#3587 =( GEOMETRIC_REPRESENTATION_CONTEXT ( 3 ) GLOBAL_UNCERTAINTY_ASSIGNED_CONTEXT ( ( #8182 ) ) GLOBAL_UNIT_ASSIGNED_CONTEXT ( ( #4572, #7156, #2146 ) ) REPRESENTATION_CONTEXT ( 'NONE', 'WORKASPACE' ) );
#3588 = AXIS2_PLACEMENT_3D ( 'NONE', #1772, #5601, #6318 ) ;
#3589 = EDGE_LOOP ( 'NONE', ( #7295, #3674, #4461, #6883 ) ) ;
#3590 = DIRECTION ( 'NONE',  ( 0.000000000000000000, 0.000000000000000000, 1.000000000000000000 ) ) ;
#3591 = FACE_BOUND ( 'NONE', #4303, .T. ) ;
#3592 = VECTOR ( 'NONE', #1405, 1000.000000000000000 ) ;
#3593 = DIRECTION ( 'NONE',  ( 0.000000000000000000, -1.000000000000000000, 0.000000000000000000 ) ) ;
#3594 = AXIS2_PLACEMENT_3D ( 'NONE', #3953, #4332, #5666 ) ;
#3595 = VERTEX_POINT ( 'NONE', #3211 ) ;
#3596 = DIRECTION ( 'NONE',  ( -0.000000000000000000, -0.000000000000000000, 1.000000000000000000 ) ) ;
#3597 = CARTESIAN_POINT ( 'NONE',  ( 0.8175244905105739646, -49.99999999999999289, -25.00000000000000355 ) ) ;
#3598 = VERTEX_POINT ( 'NONE', #5119 ) ;
#3599 = EDGE_CURVE ( 'NONE', #6111, #6896, #649, .T. ) ;
#3600 = AXIS2_PLACEMENT_3D ( 'NONE', #3310, #3391, #2700 ) ;
#3601 = CYLINDRICAL_SURFACE ( 'NONE', #504, 8.999999999999994671 ) ;
#3602 = VERTEX_POINT ( 'NONE', #5632 ) ;
#3603 = DIRECTION ( 'NONE',  ( 1.000000000000000000, 0.000000000000000000, 0.000000000000000000 ) ) ;
#3604 = CIRCLE ( 'NONE', #927, 8.999999999999994671 ) ;
#3605 = AXIS2_PLACEMENT_3D ( 'NONE', #1513, #5270, #6654 ) ;
#3606 = ORIENTED_EDGE ( 'NONE', *, *, #4699, .F. ) ;
#3607 = DIRECTION ( 'NONE',  ( 0.000000000000000000, 0.000000000000000000, -1.000000000000000000 ) ) ;
#3608 = DIRECTION ( 'NONE',  ( 0.000000000000000000, -1.000000000000000000, 1.266875999117951024E-16 ) ) ;
#3609 = ORIENTED_EDGE ( 'NONE', *, *, #7662, .T. ) ;
#3610 = ORIENTED_EDGE ( 'NONE', *, *, #2322, .F. ) ;
#3611 = CARTESIAN_POINT ( 'NONE',  ( 1.644392415218296488, 49.97938897499116706, -0.08173415109641088416 ) ) ;
#3612 = VECTOR ( 'NONE', #1170, 1000.000000000000000 ) ;
#3613 = AXIS2_PLACEMENT_3D ( 'NONE', #5955, #4646, #4686 ) ;
#3614 = EDGE_LOOP ( 'NONE', ( #2491, #1891, #3224, #1220 ) ) ;
#3615 = CARTESIAN_POINT ( 'NONE',  ( 105.0000000000000000, 72.50000000000000000, -212.5000000000000568 ) ) ;
#3616 = ORIENTED_EDGE ( 'NONE', *, *, #2080, .F. ) ;
#3617 = DIRECTION ( 'NONE',  ( 1.000000000000000000, 0.000000000000000000, 0.000000000000000000 ) ) ;
#3618 = AXIS2_PLACEMENT_3D ( 'NONE', #3496, #1074, #6850 ) ;
#3619 = DIRECTION ( 'NONE',  ( 0.000000000000000000, -1.000000000000000000, 0.000000000000000000 ) ) ;
#3620 = CONICAL_SURFACE ( 'NONE', #3459, 4.057500000000000107, 1.047197551196592746 ) ;
#3621 = EDGE_LOOP ( 'NONE', ( #3273, #1313 ) ) ;
#3622 = ORIENTED_EDGE ( 'NONE', *, *, #5152, .T. ) ;
#3623 = CARTESIAN_POINT ( 'NONE',  ( -114.9999999999999147, -115.0000000000000000, -28.00000000000002487 ) ) ;
#3624 = EDGE_LOOP ( 'NONE', ( #8047, #4455, #3673, #914 ) ) ;
#3625 = AXIS2_PLACEMENT_3D ( 'NONE', #6875, #6236, #5609 ) ;
#3626 = CARTESIAN_POINT ( 'NONE',  ( 125.0000000000000000, -52.49999999999997158, 0.000000000000000000 ) ) ;
#3627 = CARTESIAN_POINT ( 'NONE',  ( 0.000000000000000000, 4.500000000000000000, -120.5000000000000284 ) ) ;
#3628 = EDGE_CURVE ( 'NONE', #3712, #5309, #8214, .T. ) ;
#3629 = CARTESIAN_POINT ( 'NONE',  ( 99.49999999999998579, 0.000000000000000000, 0.000000000000000000 ) ) ;
#3630 = EDGE_LOOP ( 'NONE', ( #6999, #499, #3813, #1609 ) ) ;
#3631 = CARTESIAN_POINT ( 'NONE',  ( -11.38744771879169093, -48.68625849413228934, -7.328777110660809058 ) ) ;
#3632 =( NAMED_UNIT ( * ) PLANE_ANGLE_UNIT ( ) SI_UNIT ( $, .RADIAN. ) );
#3633 = ORIENTED_EDGE ( 'NONE', *, *, #7635, .F. ) ;
#3634 = ORIENTED_EDGE ( 'NONE', *, *, #3439, .F. ) ;
#3635 = EDGE_CURVE ( 'NONE', #2291, #441, #5330, .T. ) ;
#3636 = DIRECTION ( 'NONE',  ( 1.000000000000000000, 0.000000000000000000, 0.000000000000000000 ) ) ;
#3637 =( REPRESENTATION_RELATIONSHIP ('NONE','NONE', #6882, #5477 ) REPRESENTATION_RELATIONSHIP_WITH_TRANSFORMATION ( #2371 )SHAPE_REPRESENTATION_RELATIONSHIP( ) );
#3638 = EDGE_CURVE ( 'NONE', #8274, #1093, #7147, .T. ) ;
#3639 = EDGE_CURVE ( 'NONE', #8098, #3712, #7790, .T. ) ;
#3640 = DIRECTION ( 'NONE',  ( 0.000000000000000000, -0.5000000000000011102, -0.8660254037844379305 ) ) ;
#3641 = EDGE_CURVE ( 'NONE', #3478, #1112, #7228, .T. ) ;
#3642 = ORIENTED_EDGE ( 'NONE', *, *, #7323, .T. ) ;
#3643 = DIRECTION ( 'NONE',  ( -0.000000000000000000, -1.000000000000000000, 1.586032892321652236E-16 ) ) ;
#3644 = CARTESIAN_POINT ( 'NONE',  ( 5.536947881659092019, -49.69381142126947992, -23.71430020744633893 ) ) ;
#3645 = ORIENTED_EDGE ( 'NONE', *, *, #7990, .T. ) ;
#3646 = FILL_AREA_STYLE ('',( #2449 ) ) ;
#3647 = CARTESIAN_POINT ( 'NONE',  ( -55.00000000000000000, 55.00000000000000000, 240.0000000000000284 ) ) ;
#3648 = AXIS2_PLACEMENT_3D ( 'NONE', #3919, #6487, #4834 ) ;
#3649 = ADVANCED_FACE ( 'NONE', ( #2675 ), #2140, .T. ) ;
#3650 = ORIENTED_EDGE ( 'NONE', *, *, #871, .F. ) ;
#3651 = EDGE_CURVE ( 'NONE', #5704, #7049, #695, .T. ) ;
#3652 = DIRECTION ( 'NONE',  ( -1.000000000000000000, -0.000000000000000000, -0.000000000000000000 ) ) ;
#3653 = EDGE_CURVE ( 'NONE', #381, #5233, #3251, .T. ) ;
#3654 = DIRECTION ( 'NONE',  ( -1.000000000000000000, 0.000000000000000000, 0.000000000000000000 ) ) ;
#3655 = FACE_BOUND ( 'NONE', #7621, .T. ) ;
#3656 = VERTEX_POINT ( 'NONE', #3935 ) ;
#3657 = DIRECTION ( 'NONE',  ( -0.000000000000000000, -1.000000000000000000, 1.586032892321652236E-16 ) ) ;
#3658 = CARTESIAN_POINT ( 'NONE',  ( -110.0000000000000142, 115.0000000000000000, 340.0000000000000000 ) ) ;
#3659 = ORIENTED_EDGE ( 'NONE', *, *, #4069, .T. ) ;
#3660 = ITEM_DEFINED_TRANSFORMATION ( 'NONE', 'NONE', #1125,  #1299 ) ;
#3661 = EDGE_LOOP ( 'NONE', ( #2344, #845, #3681, #2107 ) ) ;
#3662 = CARTESIAN_POINT ( 'NONE',  ( 0.000000000000000000, -105.0000000000000568, 20.00000000000001776 ) ) ;
#3663 = ORIENTED_EDGE ( 'NONE', *, *, #1851, .F. ) ;
#3664 = CARTESIAN_POINT ( 'NONE',  ( 0.000000000000000000, 115.0000000000000000, 0.000000000000000000 ) ) ;
#3665 = AXIS2_PLACEMENT_3D ( 'NONE', #1526, #4643, #3438 ) ;
#3666 = ADVANCED_FACE ( 'NONE', ( #7876 ), #776, .T. ) ;
#3667 = FACE_OUTER_BOUND ( 'NONE', #433, .T. ) ;
#3668 = ADVANCED_FACE ( 'NONE', ( #1453, #2637, #1495, #4008, #6600, #1535 ), #126, .T. ) ;
#3669 = DIRECTION ( 'NONE',  ( -0.000000000000000000, -0.000000000000000000, -1.000000000000000000 ) ) ;
#3670 = CARTESIAN_POINT ( 'NONE',  ( -75.00000000000000000, -54.99999999999999289, -27.50000000000000000 ) ) ;
#3671 = EDGE_LOOP ( 'NONE', ( #8197, #1178, #6435, #2531 ) ) ;
#3672 = PRODUCT_DEFINITION_FORMATION_WITH_SPECIFIED_SOURCE ( 'ANY', '', #7957, .NOT_KNOWN. ) ;
#3673 = ORIENTED_EDGE ( 'NONE', *, *, #8169, .T. ) ;
#3674 = ORIENTED_EDGE ( 'NONE', *, *, #5796, .T. ) ;
#3675 = DIRECTION ( 'NONE',  ( -1.000000000000000000, 0.000000000000000000, 0.000000000000000000 ) ) ;
#3676 = CYLINDRICAL_SURFACE ( 'NONE', #6020, 5.999999999999991118 ) ;
#3677 = DIRECTION ( 'NONE',  ( 1.000000000000000000, 0.000000000000000000, 0.000000000000000000 ) ) ;
#3678 = VERTEX_POINT ( 'NONE', #4087 ) ;
#3679 = CARTESIAN_POINT ( 'NONE',  ( -7.620025376658135841, -49.41698073774416144, -2.582688914155140125 ) ) ;
#3680 = AXIS2_PLACEMENT_3D ( 'NONE', #3364, #8023, #2783 ) ;
#3681 = ORIENTED_EDGE ( 'NONE', *, *, #8009, .T. ) ;
#3682 = DIRECTION ( 'NONE',  ( 1.000000000000000000, 0.000000000000000000, 0.000000000000000000 ) ) ;
#3683 = DIRECTION ( 'NONE',  ( -0.000000000000000000, -0.000000000000000000, 1.000000000000000000 ) ) ;
#3684 = CIRCLE ( 'NONE', #8142, 5.999999999999991118 ) ;
#3685 = DIRECTION ( 'NONE',  ( -0.000000000000000000, -0.000000000000000000, 1.000000000000000000 ) ) ;
#3686 = ORIENTED_EDGE ( 'NONE', *, *, #1335, .T. ) ;
#3687 = PLANE ( 'NONE',  #5247 ) ;
#3688 = CARTESIAN_POINT ( 'NONE',  ( -115.0000000000000284, -115.0000000000000000, 20.00000000000000355 ) ) ;
#3689 = ADVANCED_FACE ( 'NONE', ( #4690 ), #3569, .F. ) ;
#3690 = VERTEX_POINT ( 'NONE', #2067 ) ;
#3691 =( LENGTH_UNIT ( ) NAMED_UNIT ( * ) SI_UNIT ( .MILLI., .METRE. ) );
#3692 = CARTESIAN_POINT ( 'NONE',  ( 0.000000000000000000, 0.000000000000000000, -128.0000000000000284 ) ) ;
#3693 = EDGE_CURVE ( 'NONE', #6430, #2575, #3328, .T. ) ;
#3694 = VECTOR ( 'NONE', #4751, 1000.000000000000000 ) ;
#3695 = ADVANCED_FACE ( 'NONE', ( #5877 ), #7951, .F. ) ;
#3696 = VERTEX_POINT ( 'NONE', #6637 ) ;
#3697 = UNCERTAINTY_MEASURE_WITH_UNIT (LENGTH_MEASURE( 1.000000000000000082E-05 ), #6897, 'distance_accuracy_value', 'NONE');
#3698 = VERTEX_POINT ( 'NONE', #3404 ) ;
#3699 = CARTESIAN_POINT ( 'NONE',  ( 114.9999999999999147, 115.0000000000000000, 0.000000000000000000 ) ) ;
#3700 = CARTESIAN_POINT ( 'NONE',  ( 102.5000000000000000, 1.530808498934191521E-15, -12.50000000000000000 ) ) ;
#3701 = ORIENTED_EDGE ( 'NONE', *, *, #7946, .T. ) ;
#3702 = CARTESIAN_POINT ( 'NONE',  ( 5.000000000000000000, 4.685197434473814759, -5.637851296924623057E-15 ) ) ;
#3703 = CARTESIAN_POINT ( 'NONE',  ( -125.0000000000000000, -125.0000000000000000, 0.000000000000000000 ) ) ;
#3704 = ORIENTED_EDGE ( 'NONE', *, *, #7980, .F. ) ;
#3705 = SHAPE_DEFINITION_REPRESENTATION ( #3410, #573 ) ;
#3706 = CARTESIAN_POINT ( 'NONE',  ( 12.49965553489658454, 48.41238076809164426, -11.67579978239260541 ) ) ;
#3707 = ADVANCED_FACE ( 'NONE', ( #5993 ), #6823, .F. ) ;
#3708 = PRODUCT_DEFINITION_SHAPE ( 'NONE', 'NONE',  #969 ) ;
#3709 = ORIENTED_EDGE ( 'NONE', *, *, #5048, .T. ) ;
#3710 = FACE_OUTER_BOUND ( 'NONE', #7799, .T. ) ;
#3711 = ORIENTED_EDGE ( 'NONE', *, *, #2174, .T. ) ;
#3712 = VERTEX_POINT ( 'NONE', #7840 ) ;
#3713 = DIRECTION ( 'NONE',  ( -0.000000000000000000, -0.000000000000000000, 1.000000000000000000 ) ) ;
#3714 = DIRECTION ( 'NONE',  ( -0.000000000000000000, -1.000000000000000000, 1.586032892321652236E-16 ) ) ;
#3715 = AXIS2_PLACEMENT_3D ( 'NONE', #2076, #5420, #7238 ) ;
#3716 = CARTESIAN_POINT ( 'NONE',  ( -11.23255197390108506, 48.72302474870181044, -6.955105218463160099 ) ) ;
#3717 = EDGE_CURVE ( 'NONE', #7327, #3120, #5479, .T. ) ;
#3718 = EDGE_LOOP ( 'NONE', ( #5371, #5760, #223, #2923 ) ) ;
#3719 = ORIENTED_EDGE ( 'NONE', *, *, #3585, .T. ) ;
#3720 =( NAMED_UNIT ( * ) SI_UNIT ( $, .STERADIAN. ) SOLID_ANGLE_UNIT ( ) );
#3721 = DIRECTION ( 'NONE',  ( -1.000000000000000000, 0.000000000000000000, 0.000000000000000000 ) ) ;
#3722 = FACE_OUTER_BOUND ( 'NONE', #5739, .T. ) ;
#3723 = COLOUR_RGB ( '',0.7921568627450980005, 0.8196078431372548767, 0.9333333333333333481 ) ;
#3724 = LINE ( 'NONE', #5676, #4154 ) ;
#3725 = VERTEX_POINT ( 'NONE', #6716 ) ;
#3726 = CARTESIAN_POINT ( 'NONE',  ( -9.126495132297684165, -49.16089547422079420, -21.05129937300930010 ) ) ;
#3727 = MANIFOLD_SOLID_BREP ( 'Extrude-Thin1', #5441 ) ;
#3728 = ORIENTED_EDGE ( 'NONE', *, *, #226, .F. ) ;
#3729 = CIRCLE ( 'NONE', #5885, 12.49999999999999289 ) ;
#3730 = EDGE_LOOP ( 'NONE', ( #6661, #2654, #1997, #648 ) ) ;
#3731 = DIRECTION ( 'NONE',  ( -0.000000000000000000, -0.000000000000000000, 1.000000000000000000 ) ) ;
#3732 = DIRECTION ( 'NONE',  ( -0.000000000000000000, -0.000000000000000000, -1.000000000000000000 ) ) ;
#3733 = FACE_OUTER_BOUND ( 'NONE', #2403, .T. ) ;
#3734 = VECTOR ( 'NONE', #4438, 1000.000000000000114 ) ;
#3735 = DIRECTION ( 'NONE',  ( 1.000000000000000000, 0.000000000000000000, 0.000000000000000000 ) ) ;
#3736 = CARTESIAN_POINT ( 'NONE',  ( 7.296436711415933196, -49.46595054402523317, -2.342244756090394286 ) ) ;
#3737 = CARTESIAN_POINT ( 'NONE',  ( 10.00000000000000000, 57.99999999999997868, -93.74999999999997158 ) ) ;
#3738 = CARTESIAN_POINT ( 'NONE',  ( 0.000000000000000000, -4.500000000000000000, -120.5000000000000284 ) ) ;
#3739 = VERTEX_POINT ( 'NONE', #2903 ) ;
#3740 = VECTOR ( 'NONE', #3889, 1000.000000000000000 ) ;
#3741 = AXIS2_PLACEMENT_3D ( 'NONE', #2883, #1635, #8226 ) ;
#3742 = DIRECTION ( 'NONE',  ( 1.000000000000000000, 0.000000000000000000, 0.000000000000000000 ) ) ;
#3743 = ORIENTED_EDGE ( 'NONE', *, *, #5355, .T. ) ;
#3744 = FACE_OUTER_BOUND ( 'NONE', #4171, .T. ) ;
#3745 = VERTEX_POINT ( 'NONE', #3280 ) ;
#3746 = EDGE_CURVE ( 'NONE', #6887, #4209, #4934, .T. ) ;
#3747 = CARTESIAN_POINT ( 'NONE',  ( -10.00000000000000000, -3.448762466456902719E-14, 148.7499999999999432 ) ) ;
#3748 = CARTESIAN_POINT ( 'NONE',  ( -75.00000000000000000, 75.00000000000000000, -27.50000000000000000 ) ) ;
#3749 = AXIS2_PLACEMENT_3D ( 'NONE', #3, #1929, #5027 ) ;
#3750 = CARTESIAN_POINT ( 'NONE',  ( -109.0000000000000142, 115.0000000000000000, 20.00000000000000355 ) ) ;
#3751 = ORIENTED_EDGE ( 'NONE', *, *, #6547, .T. ) ;
#3752 = APPLICATION_PROTOCOL_DEFINITION ( 'draft international standard', 'automotive_design', 1998, #6112 ) ;
#3753 = ORIENTED_EDGE ( 'NONE', *, *, #3755, .T. ) ;
#3754 = DIRECTION ( 'NONE',  ( 1.000000000000000000, 0.000000000000000000, 0.000000000000000000 ) ) ;
#3755 = EDGE_CURVE ( 'NONE', #6237, #5271, #5320, .T. ) ;
#3756 = AXIS2_PLACEMENT_3D ( 'NONE', #4230, #2939, #4276 ) ;
#3757 = AXIS2_PLACEMENT_3D ( 'NONE', #506, #2464, #3159 ) ;
#3758 = ORIENTED_EDGE ( 'NONE', *, *, #4437, .T. ) ;
#3759 = LINE ( 'NONE', #2503, #2144 ) ;
#3760 = ORIENTED_EDGE ( 'NONE', *, *, #2427, .T. ) ;
#3761 = EDGE_CURVE ( 'NONE', #3972, #7231, #2817, .T. ) ;
#3762 = PLANE ( 'NONE',  #2951 ) ;
#3763 = EDGE_CURVE ( 'NONE', #1277, #8341, #4664, .T. ) ;
#3764 = EDGE_CURVE ( 'NONE', #1618, #4405, #4117, .T. ) ;
#3765 = CIRCLE ( 'NONE', #5660, 8.999999999999994671 ) ;
#3766 = AXIS2_PLACEMENT_3D ( 'NONE', #5567, #4916, #7506 ) ;
#3767 = CARTESIAN_POINT ( 'NONE',  ( -11.85818221415417284, 48.57454970542616479, -8.462724116359975568 ) ) ;
#3768 = VERTEX_POINT ( 'NONE', #279 ) ;
#3769 = ORIENTED_EDGE ( 'NONE', *, *, #2764, .T. ) ;
#3770 = ORIENTED_EDGE ( 'NONE', *, *, #1643, .T. ) ;
#3771 = CARTESIAN_POINT ( 'NONE',  ( 0.000000000000000000, 0.000000000000000000, -250.0000000000000000 ) ) ;
#3772 = AXIS2_PLACEMENT_3D ( 'NONE', #6117, #2308, #2233 ) ;
#3773 = VECTOR ( 'NONE', #7101, 1000.000000000000000 ) ;
#3774 = FACE_OUTER_BOUND ( 'NONE', #3432, .T. ) ;
#3775 = ORIENTED_EDGE ( 'NONE', *, *, #5168, .T. ) ;
#3776 = CARTESIAN_POINT ( 'NONE',  ( -6.616553374552188949, -49.56145291835652245, -23.11303593919431165 ) ) ;
#3777 = AXIS2_PLACEMENT_3D ( 'NONE', #2673, #5249, #4006 ) ;
#3778 = EDGE_LOOP ( 'NONE', ( #7280, #446 ) ) ;
#3779 = AXIS2_PLACEMENT_3D ( 'NONE', #6581, #7903, #7260 ) ;
#3780 = ORIENTED_EDGE ( 'NONE', *, *, #3807, .T. ) ;
#3781 = DIRECTION ( 'NONE',  ( -0.000000000000000000, -1.000000000000000000, 1.586032892321652236E-16 ) ) ;
#3782 = EDGE_CURVE ( 'NONE', #2265, #2372, #1715, .T. ) ;
#3783 = CARTESIAN_POINT ( 'NONE',  ( 125.0000000000000000, -52.49999999999997158, 0.000000000000000000 ) ) ;
#3784 = CARTESIAN_POINT ( 'NONE',  ( 9.130470200569520856, -49.16013940401185067, -3.953130373342526926 ) ) ;
#3785 = CARTESIAN_POINT ( 'NONE',  ( 17.61817604250836311, 0.000000000000000000, -128.0000000000000284 ) ) ;
#3786 = PRODUCT_DEFINITION_SHAPE ( 'NONE', 'NONE',  #2672 ) ;
#3787 = FACE_OUTER_BOUND ( 'NONE', #3730, .T. ) ;
#3788 = ORIENTED_EDGE ( 'NONE', *, *, #8093, .T. ) ;
#3789 = ORIENTED_EDGE ( 'NONE', *, *, #6590, .F. ) ;
#3790 = UNCERTAINTY_MEASURE_WITH_UNIT (LENGTH_MEASURE( 1.000000000000000082E-05 ), #6519, 'distance_accuracy_value', 'NONE');
#3791 = ORIENTED_EDGE ( 'NONE', *, *, #7652, .F. ) ;
#3792 = DIRECTION ( 'NONE',  ( 1.000000000000000000, 0.000000000000000000, 0.000000000000000000 ) ) ;
#3793 = ORIENTED_EDGE ( 'NONE', *, *, #309, .T. ) ;
#3794 = DIRECTION ( 'NONE',  ( 0.000000000000000000, -0.000000000000000000, -1.000000000000000000 ) ) ;
#3795 = DIRECTION ( 'NONE',  ( -1.000000000000000000, 0.000000000000000000, 0.000000000000000000 ) ) ;
#3796 = CONTEXT_DEPENDENT_SHAPE_REPRESENTATION ( #4499, #68 ) ;
#3797 = AXIS2_PLACEMENT_3D ( 'NONE', #4538, #187, #754 ) ;
#3798 = CARTESIAN_POINT ( 'NONE',  ( 6.266608689623135220, 49.60708521373746294, -23.32352924753791967 ) ) ;
#3799 = VERTEX_POINT ( 'NONE', #3804 ) ;
#3800 = ORIENTED_EDGE ( 'NONE', *, *, #7797, .T. ) ;
#3801 = DIRECTION ( 'NONE',  ( -0.000000000000000000, -7.945337353457666666E-18, -1.000000000000000000 ) ) ;
#3802 =( NAMED_UNIT ( * ) SI_UNIT ( $, .STERADIAN. ) SOLID_ANGLE_UNIT ( ) );
#3803 = ORIENTED_EDGE ( 'NONE', *, *, #2585, .F. ) ;
#3804 = CARTESIAN_POINT ( 'NONE',  ( -105.9999999999999858, -114.9999999999999858, 10.00000000000000000 ) ) ;
#3805 = VECTOR ( 'NONE', #3027, 1000.000000000000000 ) ;
#3806 = CARTESIAN_POINT ( 'NONE',  ( 124.0000000000000000, -114.9999999999999716, 20.00000000000000000 ) ) ;
#3807 = EDGE_CURVE ( 'NONE', #8152, #4172, #5745, .T. ) ;
#3808 = VERTEX_POINT ( 'NONE', #4545 ) ;
#3809 = EDGE_CURVE ( 'NONE', #6480, #5338, #1583, .T. ) ;
#3810 = LINE ( 'NONE', #3247, #7383 ) ;
#3811 = CIRCLE ( 'NONE', #3665, 95.00000000000008527 ) ;
#3812 = DIRECTION ( 'NONE',  ( 0.000000000000000000, 1.000000000000000000, 0.000000000000000000 ) ) ;
#3813 = ORIENTED_EDGE ( 'NONE', *, *, #5462, .T. ) ;
#3814 = CARTESIAN_POINT ( 'NONE',  ( -55.00000000000000000, 55.00000000000000000, 220.0000000000000284 ) ) ;
#3815 = ORIENTED_EDGE ( 'NONE', *, *, #3761, .T. ) ;
#3816 = ADVANCED_FACE ( 'NONE', ( #4362 ), #4965, .F. ) ;
#3817 = AXIS2_PLACEMENT_3D ( 'NONE', #1903, #5006, #3742 ) ;
#3818 = ADVANCED_FACE ( 'NONE', ( #5652 ), #4798, .F. ) ;
#3819 =( GEOMETRIC_REPRESENTATION_CONTEXT ( 3 ) GLOBAL_UNCERTAINTY_ASSIGNED_CONTEXT ( ( #1007 ) ) GLOBAL_UNIT_ASSIGNED_CONTEXT ( ( #7671, #3852, #6417 ) ) REPRESENTATION_CONTEXT ( 'NONE', 'WORKASPACE' ) );
#3820 = CARTESIAN_POINT ( 'NONE',  ( -49.00000000000000711, -55.00000000000000711, -27.50000000000000000 ) ) ;
#3821 = DIRECTION ( 'NONE',  ( 1.460819769243626145E-16, -1.000000000000000000, 0.000000000000000000 ) ) ;
#3822 = FACE_OUTER_BOUND ( 'NONE', #3186, .T. ) ;
#3823 = LINE ( 'NONE', #7034, #6819 ) ;
#3824 = DIRECTION ( 'NONE',  ( -0.000000000000000000, -0.000000000000000000, -1.000000000000000000 ) ) ;
#3825 = EDGE_CURVE ( 'NONE', #2952, #7385, #6269, .T. ) ;
#3826 = VERTEX_POINT ( 'NONE', #1819 ) ;
#3827 = EDGE_CURVE ( 'NONE', #441, #7933, #1139, .T. ) ;
#3828 = ORIENTED_EDGE ( 'NONE', *, *, #2977, .T. ) ;
#3829 = ORIENTED_EDGE ( 'NONE', *, *, #1248, .F. ) ;
#3830 = CARTESIAN_POINT ( 'NONE',  ( -108.9999999999999147, -115.0000000000000000, 8.205133554287239938E-16 ) ) ;
#3831 = ORIENTED_EDGE ( 'NONE', *, *, #6013, .T. ) ;
#3832 = DIRECTION ( 'NONE',  ( -0.000000000000000000, -0.000000000000000000, -1.000000000000000000 ) ) ;
#3833 = CARTESIAN_POINT ( 'NONE',  ( 0.000000000000000000, 0.000000000000000000, 57.99999999999999289 ) ) ;
#3834 = ORIENTED_EDGE ( 'NONE', *, *, #3809, .F. ) ;
#3835 = DIRECTION ( 'NONE',  ( 0.000000000000000000, 0.000000000000000000, 1.000000000000000000 ) ) ;
#3836 = ORIENTED_EDGE ( 'NONE', *, *, #7528, .T. ) ;
#3837 = VERTEX_POINT ( 'NONE', #3018 ) ;
#3838 = FACE_OUTER_BOUND ( 'NONE', #588, .T. ) ;
#3839 = CIRCLE ( 'NONE', #4905, 20.00000000000000355 ) ;
#3840 = DIRECTION ( 'NONE',  ( 1.000000000000000000, 0.000000000000000000, 0.000000000000000000 ) ) ;
#3841 = DIRECTION ( 'NONE',  ( -0.000000000000000000, -0.000000000000000000, 1.000000000000000000 ) ) ;
#3842 = CARTESIAN_POINT ( 'NONE',  ( -3.257004588345655982, 49.90043368416229441, -24.59660869042693676 ) ) ;
#3843 = EDGE_LOOP ( 'NONE', ( #596, #1363, #7477, #5706, #5134, #4064, #4973, #6420 ) ) ;
#3844 = DIRECTION ( 'NONE',  ( 1.000000000000000000, 0.000000000000000000, 0.000000000000000000 ) ) ;
#3845 = LINE ( 'NONE', #5797, #6303 ) ;
#3846 = CYLINDRICAL_SURFACE ( 'NONE', #2607, 12.49999999999999289 ) ;
#3847 = FACE_BOUND ( 'NONE', #1243, .T. ) ;
#3848 = EDGE_CURVE ( 'NONE', #6212, #416, #5486, .T. ) ;
#3849 = VERTEX_POINT ( 'NONE', #1212 ) ;
#3850 = FACE_OUTER_BOUND ( 'NONE', #346, .T. ) ;
#3851 = EDGE_CURVE ( 'NONE', #653, #372, #3099, .T. ) ;
#3852 =( NAMED_UNIT ( * ) PLANE_ANGLE_UNIT ( ) SI_UNIT ( $, .RADIAN. ) );
#3853 = PLANE ( 'NONE',  #2266 ) ;
#3854 = ORIENTED_EDGE ( 'NONE', *, *, #5451, .T. ) ;
#3855 = CIRCLE ( 'NONE', #5473, 5.999999999999991118 ) ;
#3856 = DIRECTION ( 'NONE',  ( -1.000000000000000000, -0.000000000000000000, -0.000000000000000000 ) ) ;
#3857 = VECTOR ( 'NONE', #4468, 1000.000000000000000 ) ;
#3858 = DIRECTION ( 'NONE',  ( 0.000000000000000000, 1.000000000000000000, 0.000000000000000000 ) ) ;
#3859 = ADVANCED_FACE ( 'NONE', ( #1979 ), #3853, .F. ) ;
#3860 = CARTESIAN_POINT ( 'NONE',  ( 0.000000000000000000, -49.99999999999999289, 0.000000000000000000 ) ) ;
#3861 = DIRECTION ( 'NONE',  ( -0.000000000000000000, -0.000000000000000000, -1.000000000000000000 ) ) ;
#3862=STYLED_ITEM('',(#8407),#3727);
#3863 = DIRECTION ( 'NONE',  ( -0.000000000000000000, -0.000000000000000000, 1.000000000000000000 ) ) ;
#3864 = VERTEX_POINT ( 'NONE', #2509 ) ;
#3865 = VECTOR ( 'NONE', #3006, 1000.000000000000000 ) ;
#3866 = EDGE_LOOP ( 'NONE', ( #5583, #6325, #7669, #2624 ) ) ;
#3867 = VERTEX_POINT ( 'NONE', #1925 ) ;
#3868 = DIRECTION ( 'NONE',  ( -0.000000000000000000, -0.000000000000000000, 1.000000000000000000 ) ) ;
#3869 = CYLINDRICAL_SURFACE ( 'NONE', #7339, 5.999999999999991118 ) ;
#3870 = ORIENTED_EDGE ( 'NONE', *, *, #2487, .F. ) ;
#3871 = CARTESIAN_POINT ( 'NONE',  ( 0.000000000000000000, 0.000000000000000000, 35.00000000000000000 ) ) ;
#3872 = CARTESIAN_POINT ( 'NONE',  ( 110.0000000000000142, -115.0000000000000000, 340.0000000000000000 ) ) ;
#3873 = EDGE_CURVE ( 'NONE', #3094, #66, #4336, .T. ) ;
#3874 = LINE ( 'NONE', #1954, #260 ) ;
#3875 = EDGE_LOOP ( 'NONE', ( #8335, #996, #4449, #7820 ) ) ;
#3876 = AXIS2_PLACEMENT_3D ( 'NONE', #5645, #8270, #622 ) ;
#3877 = ORIENTED_EDGE ( 'NONE', *, *, #6123, .T. ) ;
#3878 = LINE ( 'NONE', #2093, #738 ) ;
#3879 = DIRECTION ( 'NONE',  ( 0.000000000000000000, 0.000000000000000000, -1.000000000000000000 ) ) ;
#3880 = CIRCLE ( 'NONE', #1727, 5.499999999999991118 ) ;
#3881 = ORIENTED_EDGE ( 'NONE', *, *, #5404, .T. ) ;
#3882 = LINE ( 'NONE', #597, #1761 ) ;
#3883 = ADVANCED_FACE ( 'NONE', ( #5068 ), #3182, .F. ) ;
#3884 = VECTOR ( 'NONE', #1470, 1000.000000000000000 ) ;
#3885 = ORIENTED_EDGE ( 'NONE', *, *, #6072, .F. ) ;
#3886 = DIRECTION ( 'NONE',  ( 0.000000000000000000, 0.000000000000000000, 1.000000000000000000 ) ) ;
#3887 = AXIS2_PLACEMENT_3D ( 'NONE', #7785, #6584, #3962 ) ;
#3888 = FACE_BOUND ( 'NONE', #16, .T. ) ;
#3889 = DIRECTION ( 'NONE',  ( 0.000000000000000000, 1.000000000000000000, -0.000000000000000000 ) ) ;
#3890 = CARTESIAN_POINT ( 'NONE',  ( -1.380900529026471473E-13, -12.49999999999999467, -54.99999999999998579 ) ) ;
#3891 = CIRCLE ( 'NONE', #1338, 14.99999999999998579 ) ;
#3892 = VECTOR ( 'NONE', #5732, 1000.000000000000000 ) ;
#3893 = CARTESIAN_POINT ( 'NONE',  ( 95.00000000000002842, -95.00000000000002842, 35.00000000000000000 ) ) ;
#3894 = ORIENTED_EDGE ( 'NONE', *, *, #7029, .T. ) ;
#3895 = DIRECTION ( 'NONE',  ( 0.000000000000000000, 1.000000000000000000, -1.460819769243626884E-16 ) ) ;
#3896 = DIRECTION ( 'NONE',  ( 1.293760902945442121E-31, -1.874743562255115479E-31, 0.9999999999999998890 ) ) ;
#3897 = ORIENTED_EDGE ( 'NONE', *, *, #2452, .T. ) ;
#3898 = ORIENTED_EDGE ( 'NONE', *, *, #4753, .F. ) ;
#3899 = VECTOR ( 'NONE', #532, 1000.000000000000000 ) ;
#3900 = CONICAL_SURFACE ( 'NONE', #7549, 6.999999999999999112, 0.7853981633974482790 ) ;
#3901 = CARTESIAN_POINT ( 'NONE',  ( 0.000000000000000000, 0.000000000000000000, 57.99999999999999289 ) ) ;
#3902 = CARTESIAN_POINT ( 'NONE',  ( -115.0000000000000000, -115.0000000000000000, 270.0000000000000000 ) ) ;
#3903 = CYLINDRICAL_SURFACE ( 'NONE', #4427, 12.50000000000000000 ) ;
#3904 = AXIS2_PLACEMENT_3D ( 'NONE', #2269, #7410, #1625 ) ;
#3905 = CARTESIAN_POINT ( 'NONE',  ( -1.173433385984108997E-13, 12.50000000000001066, -12.50000000000001421 ) ) ;
#3906 = CIRCLE ( 'NONE', #7697, 12.50000000000000000 ) ;
#3907 = CARTESIAN_POINT ( 'NONE',  ( -124.0000000000000000, -114.9999999999999858, 20.00000000000000000 ) ) ;
#3908 = ORIENTED_EDGE ( 'NONE', *, *, #3639, .F. ) ;
#3909 = EDGE_CURVE ( 'NONE', #4158, #6525, #6293, .T. ) ;
#3910 = EDGE_CURVE ( 'NONE', #5894, #4086, #4278, .T. ) ;
#3911 = VECTOR ( 'NONE', #6678, 1000.000000000000000 ) ;
#3912 = EDGE_LOOP ( 'NONE', ( #1444, #2353, #4457, #6555 ) ) ;
#3913 = DIRECTION ( 'NONE',  ( 0.000000000000000000, -0.000000000000000000, -1.000000000000000000 ) ) ;
#3914 = VECTOR ( 'NONE', #1649, 1000.000000000000000 ) ;
#3915 = VERTEX_POINT ( 'NONE', #7904 ) ;
#3916 = CARTESIAN_POINT ( 'NONE',  ( 0.000000000000000000, -2.342598717236898054, 4.057500000000003659 ) ) ;
#3917 = DIRECTION ( 'NONE',  ( 0.000000000000000000, 1.000000000000000000, 0.000000000000000000 ) ) ;
#3918 = ITEM_DEFINED_TRANSFORMATION ( 'NONE', 'NONE', #6093,  #1299 ) ;
#3919 = CARTESIAN_POINT ( 'NONE',  ( -1.110223024625156540E-13, -12.50000000000001066, 1.387778780781445676E-14 ) ) ;
#3920 = EDGE_CURVE ( 'NONE', #8240, #4180, #4345, .T. ) ;
#3921 = PRODUCT_DEFINITION_SHAPE ( 'NONE', 'NONE',  #8358 ) ;
#3922 = DIRECTION ( 'NONE',  ( 0.000000000000000000, 1.000000000000000000, 0.000000000000000000 ) ) ;
#3923 = FACE_OUTER_BOUND ( 'NONE', #3487, .T. ) ;
#3924 = VERTEX_POINT ( 'NONE', #889 ) ;
#3925 =( REPRESENTATION_RELATIONSHIP ('NONE','NONE', #6882, #239 ) REPRESENTATION_RELATIONSHIP_WITH_TRANSFORMATION ( #1390 )SHAPE_REPRESENTATION_RELATIONSHIP( ) );
#3926 = DIRECTION ( 'NONE',  ( 1.000000000000000000, 0.000000000000000000, 0.000000000000000000 ) ) ;
#3927 = ORIENTED_EDGE ( 'NONE', *, *, #5378, .F. ) ;
#3928 = DIRECTION ( 'NONE',  ( 1.000000000000000000, 0.000000000000000000, 0.000000000000000000 ) ) ;
#3929 = DIRECTION ( 'NONE',  ( -0.000000000000000000, -0.000000000000000000, 1.000000000000000000 ) ) ;
#3930 = EDGE_CURVE ( 'NONE', #8339, #6651, #3729, .T. ) ;
#3931 = CARTESIAN_POINT ( 'NONE',  ( 115.0000000000000000, 115.0000000000000000, 270.0000000000000000 ) ) ;
#3932 = DIRECTION ( 'NONE',  ( 0.000000000000000000, 1.000000000000000000, -1.460819769243626884E-16 ) ) ;
#3933 = DIRECTION ( 'NONE',  ( 0.000000000000000000, 0.000000000000000000, -1.000000000000000000 ) ) ;
#3934 = VERTEX_POINT ( 'NONE', #4864 ) ;
#3935 = CARTESIAN_POINT ( 'NONE',  ( -75.00000000000001421, 0.000000000000000000, 20.00000000000000355 ) ) ;
#3936 = CARTESIAN_POINT ( 'NONE',  ( 1.507722968250244105E-14, -91.25000000000000000, -188.2499999999999147 ) ) ;
#3937 = PLANE ( 'NONE',  #1599 ) ;
#3938 = ORIENTED_EDGE ( 'NONE', *, *, #7686, .T. ) ;
#3939 = CARTESIAN_POINT ( 'NONE',  ( 1.592040838891559490E-15, 125.0000000000000568, 92.99999999999992895 ) ) ;
#3940 = DIRECTION ( 'NONE',  ( -1.000000000000000000, 0.000000000000000000, 0.000000000000000000 ) ) ;
#3941 = CARTESIAN_POINT ( 'NONE',  ( -125.0000000000000000, 125.0000000000000000, 0.000000000000000000 ) ) ;
#3942 =( NAMED_UNIT ( * ) PLANE_ANGLE_UNIT ( ) SI_UNIT ( $, .RADIAN. ) );
#3943 = CIRCLE ( 'NONE', #6091, 2.499999999999996003 ) ;
#3944 =( NAMED_UNIT ( * ) SI_UNIT ( $, .STERADIAN. ) SOLID_ANGLE_UNIT ( ) );
#3945 = AXIS2_PLACEMENT_3D ( 'NONE', #3252, #696, #4994 ) ;
#3946 = ORIENTED_EDGE ( 'NONE', *, *, #2757, .T. ) ;
#3947 = DIRECTION ( 'NONE',  ( -9.992007221626408864E-16, -1.000000000000000000, 0.000000000000000000 ) ) ;
#3948 = ORIENTED_EDGE ( 'NONE', *, *, #3376, .T. ) ;
#3949 = CARTESIAN_POINT ( 'NONE',  ( 5.000000000000000000, 7.027796151710712813, -4.057500000000006324 ) ) ;
#3950 = EDGE_CURVE ( 'NONE', #7585, #805, #5925, .T. ) ;
#3951 = EDGE_LOOP ( 'NONE', ( #2661, #1232, #5887 ) ) ;
#3952 = CARTESIAN_POINT ( 'NONE',  ( -120.0000000000000000, 115.0000000000000000, 340.0000000000000000 ) ) ;
#3953 = CARTESIAN_POINT ( 'NONE',  ( 5.000000000000000000, -2.342598717236898054, 4.057500000000003659 ) ) ;
#3954 = EDGE_CURVE ( 'NONE', #5855, #7385, #4389, .T. ) ;
#3955 = DIRECTION ( 'NONE',  ( -0.000000000000000000, -0.000000000000000000, 1.000000000000000000 ) ) ;
#3956 = AXIS2_PLACEMENT_3D ( 'NONE', #1158, #2997, #1202 ) ;
#3957 = CARTESIAN_POINT ( 'NONE',  ( 99.49999999999998579, 0.000000000000000000, 0.000000000000000000 ) ) ;
#3958 = ORIENTED_EDGE ( 'NONE', *, *, #6646, .F. ) ;
#3959 = CARTESIAN_POINT ( 'NONE',  ( -75.00000000000000000, 0.000000000000000000, 0.000000000000000000 ) ) ;
#3960 = AXIS2_PLACEMENT_3D ( 'NONE', #3977, #782, #7881 ) ;
#3961 = EDGE_CURVE ( 'NONE', #3000, #306, #1315, .T. ) ;
#3962 = DIRECTION ( 'NONE',  ( -1.000000000000000000, 0.000000000000000000, 0.000000000000000000 ) ) ;
#3963 = CIRCLE ( 'NONE', #7346, 49.99999999999998579 ) ;
#3964 = EDGE_LOOP ( 'NONE', ( #2333, #1762, #6916, #4576 ) ) ;
#3965 = SHAPE_REPRESENTATION ( 'Timing Pulley', ( #1299 ), #6550 ) ;
#3966 = FACE_BOUND ( 'NONE', #1349, .T. ) ;
#3967 = LINE ( 'NONE', #6545, #3452 ) ;
#3968 = DIRECTION ( 'NONE',  ( 0.000000000000000000, -1.000000000000000000, 0.000000000000000000 ) ) ;
#3969 = CYLINDRICAL_SURFACE ( 'NONE', #4703, 5.999999999999991118 ) ;
#3970 = FACE_OUTER_BOUND ( 'NONE', #4590, .T. ) ;
#3971 = DIRECTION ( 'NONE',  ( 0.000000000000000000, -1.000000000000000000, 1.586032892321652236E-16 ) ) ;
#3972 = VERTEX_POINT ( 'NONE', #2480 ) ;
#3973 = DIRECTION ( 'NONE',  ( 1.000000000000000000, 0.000000000000000000, 0.000000000000000000 ) ) ;
#3974 = ORIENTED_EDGE ( 'NONE', *, *, #4192, .F. ) ;
#3975 = VECTOR ( 'NONE', #6251, 1000.000000000000000 ) ;
#3976 = DIRECTION ( 'NONE',  ( 0.000000000000000000, 0.000000000000000000, 1.000000000000000000 ) ) ;
#3977 = CARTESIAN_POINT ( 'NONE',  ( 55.00000000000000000, -55.00000000000000000, 220.0000000000000284 ) ) ;
#3978 = SURFACE_STYLE_USAGE ( .BOTH. , #132 ) ;
#3979 = DIRECTION ( 'NONE',  ( -0.000000000000000000, -0.000000000000000000, 1.000000000000000000 ) ) ;
#3980 = AXIS2_PLACEMENT_3D ( 'NONE', #7921, #2755, #7997 ) ;
#3981 = PLANE ( 'NONE',  #3158 ) ;
#3982 = VERTEX_POINT ( 'NONE', #4866 ) ;
#3983 = CYLINDRICAL_SURFACE ( 'NONE', #6229, 5.999999999999991118 ) ;
#3984 = CYLINDRICAL_SURFACE ( 'NONE', #6042, 8.999999999999994671 ) ;
#3985 = DIRECTION ( 'NONE',  ( -1.752490724247359037E-17, 1.000000000000000000, 3.853078496550133260E-17 ) ) ;
#3986 = VERTEX_POINT ( 'NONE', #4216 ) ;
#3987 = CARTESIAN_POINT ( 'NONE',  ( -55.00000000000000000, -55.00000000000000000, 240.0000000000000284 ) ) ;
#3988 = LINE ( 'NONE', #2846, #5362 ) ;
#3989 = LINE ( 'NONE', #3353, #5140 ) ;
#3990 = ORIENTED_EDGE ( 'NONE', *, *, #226, .T. ) ;
#3991 = EDGE_CURVE ( 'NONE', #4671, #7451, #7586, .T. ) ;
#3992 = DIRECTION ( 'NONE',  ( -1.000000000000000000, -0.000000000000000000, -0.000000000000000000 ) ) ;
#3993 = ORIENTED_EDGE ( 'NONE', *, *, #8247, .F. ) ;
#3994 = CONICAL_SURFACE ( 'NONE', #219, 4.999999999999990230, 1.029744258676653201 ) ;
#3995 = VECTOR ( 'NONE', #5726, 1000.000000000000000 ) ;
#3996 = CARTESIAN_POINT ( 'NONE',  ( 49.00000000000000000, 55.00000000000000711, 27.50000000000000000 ) ) ;
#3997 = CARTESIAN_POINT ( 'NONE',  ( 55.00000000000000711, 54.99999999999999289, -27.50000000000000000 ) ) ;
#3998 = ORIENTED_EDGE ( 'NONE', *, *, #980, .F. ) ;
#3999 = VECTOR ( 'NONE', #1194, 1000.000000000000000 ) ;
#4000 = ADVANCED_FACE ( 'NONE', ( #1036, #2920, #3591, #2396, #5680, #1764 ), #1712, .T. ) ;
#4001 = ADVANCED_FACE ( 'NONE', ( #4906 ), #1843, .F. ) ;
#4002 = CARTESIAN_POINT ( 'NONE',  ( 109.0000000000000142, 115.0000000000000000, 20.00000000000000355 ) ) ;
#4003 = AXIS2_PLACEMENT_3D ( 'NONE', #3508, #487, #6223 ) ;
#4004 = FACE_OUTER_BOUND ( 'NONE', #6458, .T. ) ;
#4005 = DIRECTION ( 'NONE',  ( -0.000000000000000000, -0.000000000000000000, 1.000000000000000000 ) ) ;
#4006 = DIRECTION ( 'NONE',  ( 0.000000000000000000, 0.000000000000000000, 1.000000000000000000 ) ) ;
#4007 = ORIENTED_EDGE ( 'NONE', *, *, #3950, .F. ) ;
#4008 = FACE_BOUND ( 'NONE', #2211, .T. ) ;
#4009 = DIRECTION ( 'NONE',  ( -0.000000000000000000, -0.000000000000000000, 1.000000000000000000 ) ) ;
#4010 = ORIENTED_EDGE ( 'NONE', *, *, #2822, .T. ) ;
#4011 = DIRECTION ( 'NONE',  ( -0.000000000000000000, -0.000000000000000000, 1.000000000000000000 ) ) ;
#4012 = VERTEX_POINT ( 'NONE', #5035 ) ;
#4013 = DIRECTION ( 'NONE',  ( -0.000000000000000000, -0.000000000000000000, 1.000000000000000000 ) ) ;
#4014 = VECTOR ( 'NONE', #6749, 1000.000000000000000 ) ;
#4015 = CIRCLE ( 'NONE', #4274, 3.000000000000001776 ) ;
#4016 = PLANE ( 'NONE',  #5322 ) ;
#4017 = LINE ( 'NONE', #2074, #2950 ) ;
#4018 = FACE_BOUND ( 'NONE', #6888, .T. ) ;
#4019 = VECTOR ( 'NONE', #6055, 1000.000000000000000 ) ;
#4020 = VECTOR ( 'NONE', #3685, 1000.000000000000000 ) ;
#4021 = VERTEX_POINT ( 'NONE', #6860 ) ;
#4022 = LINE ( 'NONE', #2842, #719 ) ;
#4023 = EDGE_CURVE ( 'NONE', #7555, #7110, #1177, .T. ) ;
#4024 = EDGE_CURVE ( 'NONE', #6262, #2853, #8040, .T. ) ;
#4025 = FACE_BOUND ( 'NONE', #1632, .T. ) ;
#4026 = VECTOR ( 'NONE', #93, 1000.000000000000000 ) ;
#4027 = CIRCLE ( 'NONE', #4428, 8.999999999999994671 ) ;
#4028 = DIRECTION ( 'NONE',  ( 0.000000000000000000, 1.000000000000000000, -0.000000000000000000 ) ) ;
#4029 = PLANE ( 'NONE',  #2811 ) ;
#4030 = LINE ( 'NONE', #5003, #2544 ) ;
#4031 = DIRECTION ( 'NONE',  ( -0.000000000000000000, -0.000000000000000000, 1.000000000000000000 ) ) ;
#4032 = AXIS2_PLACEMENT_3D ( 'NONE', #1778, #4127, #2785 ) ;
#4033 = ORIENTED_EDGE ( 'NONE', *, *, #3910, .T. ) ;
#4034 = ORIENTED_EDGE ( 'NONE', *, *, #3930, .F. ) ;
#4035 = CARTESIAN_POINT ( 'NONE',  ( -120.0000000000000000, 125.0000000000000000, 0.000000000000000000 ) ) ;
#4036 = ORIENTED_EDGE ( 'NONE', *, *, #2588, .T. ) ;
#4037 = CARTESIAN_POINT ( 'NONE',  ( -31.74999999999995737, 9.797174393178825657E-16, -8.000000000000000000 ) ) ;
#4038 = CARTESIAN_POINT ( 'NONE',  ( 75.00000000000000000, -75.00000000000000000, 27.50000000000000000 ) ) ;
#4039 = CARTESIAN_POINT ( 'NONE',  ( 0.000000000000000000, 2.499999999999984013, -246.6833752096445664 ) ) ;
#4040 = CYLINDRICAL_SURFACE ( 'NONE', #5636, 20.00000000000000355 ) ;
#4041 = DIRECTION ( 'NONE',  ( 0.000000000000000000, -1.000000000000000000, 0.000000000000000000 ) ) ;
#4042 = CARTESIAN_POINT ( 'NONE',  ( -10.00000000000000000, 57.99999999999990052, 93.75000000000004263 ) ) ;
#4043 = PRODUCT_RELATED_PRODUCT_CATEGORY ( 'part', '', ( #7894 ) ) ;
#4044 = DIRECTION ( 'NONE',  ( 0.000000000000000000, 0.000000000000000000, -1.000000000000000000 ) ) ;
#4045 = ORIENTED_EDGE ( 'NONE', *, *, #2298, .F. ) ;
#4046 = CARTESIAN_POINT ( 'NONE',  ( 115.0000000000000000, 115.0000000000000000, 340.0000000000000000 ) ) ;
#4047 = EDGE_CURVE ( 'NONE', #210, #8056, #6564, .T. ) ;
#4048 = CARTESIAN_POINT ( 'NONE',  ( 0.000000000000000000, 9.184850993605147944E-16, 6.999999999999999112 ) ) ;
#4049 = EDGE_CURVE ( 'NONE', #7975, #6953, #2965, .T. ) ;
#4051 = ORIENTED_EDGE ( 'NONE', *, *, #3638, .F. ) ;
#4050 = CIRCLE ( 'NONE', #277, 12.50000000000000000 ) ;
#4052 = ORIENTED_EDGE ( 'NONE', *, *, #1533, .T. ) ;
#4053 = FACE_BOUND ( 'NONE', #2051, .T. ) ;
#4054 = PLANE ( 'NONE',  #2355 ) ;
#4055 = CYLINDRICAL_SURFACE ( 'NONE', #390, 5.999999999999991118 ) ;
#4056 = CARTESIAN_POINT ( 'NONE',  ( 0.000000000000000000, 0.000000000000000000, 0.000000000000000000 ) ) ;
#4057 = DIRECTION ( 'NONE',  ( 1.000000000000000000, 0.000000000000000000, 0.000000000000000000 ) ) ;
#4058 = EDGE_CURVE ( 'NONE', #1522, #3867, #5553, .T. ) ;
#4059 = DIRECTION ( 'NONE',  ( 0.000000000000000000, 1.000000000000000000, -1.295896757998781966E-15 ) ) ;
#4060 = CYLINDRICAL_SURFACE ( 'NONE', #3316, 9.000000000000007105 ) ;
#4061 = VECTOR ( 'NONE', #2800, 1000.000000000000000 ) ;
#4062 = ORIENTED_EDGE ( 'NONE', *, *, #5426, .F. ) ;
#4063 = DIRECTION ( 'NONE',  ( -0.000000000000000000, -0.000000000000000000, -1.000000000000000000 ) ) ;
#4064 = ORIENTED_EDGE ( 'NONE', *, *, #4299, .T. ) ;
#4065 = CARTESIAN_POINT ( 'NONE',  ( 5.000000000000000000, -3.513898075855361292, -2.028749999999992504 ) ) ;
#4066 = CIRCLE ( 'NONE', #8273, 9.000000000000007105 ) ;
#4067 = CARTESIAN_POINT ( 'NONE',  ( 14.14213562373095279, -5.000000000000000000, 57.99999999999999289 ) ) ;
#4068 = AXIS2_PLACEMENT_3D ( 'NONE', #6302, #127, #1608 ) ;
#4069 = EDGE_CURVE ( 'NONE', #7451, #984, #3548, .T. ) ;
#4070 = DIRECTION ( 'NONE',  ( -0.000000000000000000, -0.000000000000000000, 1.000000000000000000 ) ) ;
#4071 =( REPRESENTATION_RELATIONSHIP ('NONE','NONE', #6882, #239 ) REPRESENTATION_RELATIONSHIP_WITH_TRANSFORMATION ( #3153 )SHAPE_REPRESENTATION_RELATIONSHIP( ) );
#4072 = VERTEX_POINT ( 'NONE', #5596 ) ;
#4073 = ADVANCED_FACE ( 'NONE', ( #8173 ), #5513, .F. ) ;
#4074 = EDGE_LOOP ( 'NONE', ( #4626, #7759, #7468, #4207, #6058 ) ) ;
#4075 = DIRECTION ( 'NONE',  ( 0.000000000000000000, 0.000000000000000000, -1.000000000000000000 ) ) ;
#4076 = VERTEX_POINT ( 'NONE', #6260 ) ;
#4077 = CARTESIAN_POINT ( 'NONE',  ( 102.5000000000000000, 1.530808498934191521E-15, -12.50000000000000000 ) ) ;
#4078 = DIRECTION ( 'NONE',  ( 0.000000000000000000, 1.632680918566406547E-16, -1.000000000000000000 ) ) ;
#4079 = AXIS2_PLACEMENT_3D ( 'NONE', #5210, #91, #2073 ) ;
#4080 = DIRECTION ( 'NONE',  ( -1.000000000000000000, 0.000000000000000000, -0.000000000000000000 ) ) ;
#4081 = PLANE ( 'NONE',  #5370 ) ;
#4082 = FACE_BOUND ( 'NONE', #6380, .T. ) ;
#4083 = CARTESIAN_POINT ( 'NONE',  ( 10.00000000000000000, -55.00000000000000711, 93.74999999999998579 ) ) ;
#4084 = CARTESIAN_POINT ( 'NONE',  ( 75.00000000000000000, 1.530808498934191521E-15, -12.50000000000000000 ) ) ;
#4085 = VERTEX_POINT ( 'NONE', #8262 ) ;
#4086 = VERTEX_POINT ( 'NONE', #3049 ) ;
#4087 = CARTESIAN_POINT ( 'NONE',  ( 1.000000000000000888, 0.000000000000000000, -8.000000000000000000 ) ) ;
#4088 = ORIENTED_EDGE ( 'NONE', *, *, #2172, .F. ) ;
#4089 = CYLINDRICAL_SURFACE ( 'NONE', #6569, 12.50000000000000000 ) ;
#4090 = MECHANICAL_DESIGN_GEOMETRIC_PRESENTATION_REPRESENTATION (  '', ( #5733 ), #8020 ) ;
#4091 = EDGE_CURVE ( 'NONE', #354, #5976, #7375, .T. ) ;
#4092 = EDGE_CURVE ( 'NONE', #7828, #431, #4999, .T. ) ;
#4093 = DIRECTION ( 'NONE',  ( 0.000000000000000000, 1.000000000000000000, 0.000000000000000000 ) ) ;
#4094 = FACE_OUTER_BOUND ( 'NONE', #571, .T. ) ;
#4095 = DIRECTION ( 'NONE',  ( 0.000000000000000000, -0.000000000000000000, -1.000000000000000000 ) ) ;
#4096 = DIRECTION ( 'NONE',  ( 0.000000000000000000, 0.000000000000000000, -1.000000000000000000 ) ) ;
#4097 = ORIENTED_EDGE ( 'NONE', *, *, #1484, .F. ) ;
#4098 = CARTESIAN_POINT ( 'NONE',  ( 5.000000000000000000, 5.258101095580058680E-15, 4.057500000000000995 ) ) ;
#4099 = ADVANCED_FACE ( 'NONE', ( #6309 ), #2530, .F. ) ;
#4100 = EDGE_CURVE ( 'NONE', #4405, #6401, #1039, .T. ) ;
#4101 = CARTESIAN_POINT ( 'NONE',  ( -109.4999999999999858, 114.9999999999999858, 0.000000000000000000 ) ) ;
#4102 = ORIENTED_EDGE ( 'NONE', *, *, #2788, .T. ) ;
#4103 = CARTESIAN_POINT ( 'NONE',  ( -114.9999999999999147, 0.000000000000000000, 250.0000000000000000 ) ) ;
#4104 = VERTEX_POINT ( 'NONE', #1332 ) ;
#4105 = CARTESIAN_POINT ( 'NONE',  ( -114.9999999999999858, -114.9999999999999858, 0.000000000000000000 ) ) ;
#4106 = FACE_OUTER_BOUND ( 'NONE', #6567, .T. ) ;
#4107 = AXIS2_PLACEMENT_3D ( 'NONE', #2522, #1898, #5172 ) ;
#4108 = CARTESIAN_POINT ( 'NONE',  ( 10.00000000000000000, -58.00000000000000711, 93.74999999999998579 ) ) ;
#4109 = LINE ( 'NONE', #6096, #2197 ) ;
#4110 = EDGE_LOOP ( 'NONE', ( #4975, #3111, #2600, #1062, #5216, #6224, #7734, #1974 ) ) ;
#4111 = VECTOR ( 'NONE', #261, 1000.000000000000000 ) ;
#4112 = PRODUCT_DEFINITION_CONTEXT ( 'detailed design', #7435, 'design' ) ;
#4113 = ORIENTED_EDGE ( 'NONE', *, *, #1647, .F. ) ;
#4114 = CARTESIAN_POINT ( 'NONE',  ( 0.000000000000000000, 105.0000000000000426, 66.99999999999992895 ) ) ;
#4115 = ORIENTED_EDGE ( 'NONE', *, *, #7990, .F. ) ;
#4116 = CARTESIAN_POINT ( 'NONE',  ( 55.00000000000000711, 75.00000000000000000, -27.50000000000000000 ) ) ;
#4117 = LINE ( 'NONE', #934, #4670 ) ;
#4118 = AXIS2_PLACEMENT_3D ( 'NONE', #5841, #7795, #2711 ) ;
#4119 = EDGE_LOOP ( 'NONE', ( #2934, #4793, #6479 ) ) ;
#4120 = LINE ( 'NONE', #6150, #2190 ) ;
#4121 = FACE_OUTER_BOUND ( 'NONE', #7722, .T. ) ;
#4122 = EDGE_CURVE ( 'NONE', #5539, #6702, #6148, .T. ) ;
#4123 = CARTESIAN_POINT ( 'NONE',  ( -114.9999999999999716, 114.9999999999999858, 0.000000000000000000 ) ) ;
#4124 = AXIS2_PLACEMENT_3D ( 'NONE', #6919, #6956, #1095 ) ;
#4125 = CARTESIAN_POINT ( 'NONE',  ( 0.000000000000000000, 0.000000000000000000, 240.0000000000000284 ) ) ;
#4126 = CYLINDRICAL_SURFACE ( 'NONE', #3613, 15.00000000000001421 ) ;
#4127 = DIRECTION ( 'NONE',  ( 1.000000000000000000, 0.000000000000000000, 0.000000000000000000 ) ) ;
#4128 = ORIENTED_EDGE ( 'NONE', *, *, #3653, .T. ) ;
#4129 = AXIS2_PLACEMENT_3D ( 'NONE', #5629, #2267, #4988 ) ;
#4130 = VECTOR ( 'NONE', #7929, 1000.000000000000000 ) ;
#4131 = DIRECTION ( 'NONE',  ( -0.5000000000000042188, 0.000000000000000000, 0.8660254037844361541 ) ) ;
#4132 = CIRCLE ( 'NONE', #516, 54.99999999999996447 ) ;
#4133 = DIRECTION ( 'NONE',  ( -0.000000000000000000, -0.000000000000000000, -1.000000000000000000 ) ) ;
#4134 = LINE ( 'NONE', #5418, #5387 ) ;
#4135 = ORIENTED_EDGE ( 'NONE', *, *, #1806, .T. ) ;
#4136 = DIRECTION ( 'NONE',  ( -1.000000000000000000, -0.000000000000000000, -0.000000000000000000 ) ) ;
#4137 = SHAPE_REPRESENTATION_RELATIONSHIP ( 'NONE' , 'NONE' ,  #1440, #6626 ) ;
#4138 = CYLINDRICAL_SURFACE ( 'NONE', #3980, 4.999999999999990230 ) ;
#4139 = LINE ( 'NONE', #2797, #1322 ) ;
#4140 = ORIENTED_EDGE ( 'NONE', *, *, #6373, .F. ) ;
#4141 = VECTOR ( 'NONE', #4586, 1000.000000000000000 ) ;
#4142 = AXIS2_PLACEMENT_3D ( 'NONE', #2288, #7432, #449 ) ;
#4143 = DIRECTION ( 'NONE',  ( -1.000000000000000000, -0.000000000000000000, -0.000000000000000000 ) ) ;
#4144 = ORIENTED_EDGE ( 'NONE', *, *, #3375, .T. ) ;
#4145 = CARTESIAN_POINT ( 'NONE',  ( -125.0000000000000000, 52.50000000000000000, 190.0000000000000284 ) ) ;
#4146 = CARTESIAN_POINT ( 'NONE',  ( -114.9999999999999858, -114.9999999999999858, 20.00000000000000000 ) ) ;
#4147 = PRODUCT_DEFINITION ( 'UNKNOWN', '', #3524, #2933 ) ;
#4148 = AXIS2_PLACEMENT_3D ( 'NONE', #6948, #1130, #3858 ) ;
#4149 =( NAMED_UNIT ( * ) SI_UNIT ( $, .STERADIAN. ) SOLID_ANGLE_UNIT ( ) );
#4150 = DIRECTION ( 'NONE',  ( -0.000000000000000000, -0.000000000000000000, 1.000000000000000000 ) ) ;
#4151 = EDGE_CURVE ( 'NONE', #4528, #8051, #5759, .T. ) ;
#4152 = EDGE_CURVE ( 'NONE', #4329, #2735, #3294, .T. ) ;
#4153 = ORIENTED_EDGE ( 'NONE', *, *, #5585, .T. ) ;
#4154 = VECTOR ( 'NONE', #8253, 1000.000000000000000 ) ;
#4155 = AXIS2_PLACEMENT_3D ( 'NONE', #6677, #4765, #2863 ) ;
#4156 = EDGE_LOOP ( 'NONE', ( #3081, #4415, #4356 ) ) ;
#4157 = CARTESIAN_POINT ( 'NONE',  ( 115.0000000000000000, -114.9999999999999716, 20.00000000000000000 ) ) ;
#4158 = VERTEX_POINT ( 'NONE', #8 ) ;
#4159 = CARTESIAN_POINT ( 'NONE',  ( 114.9999999999999858, 115.0000000000000000, 16.39483628583463570 ) ) ;
#4160 = DIRECTION ( 'NONE',  ( 0.000000000000000000, 0.000000000000000000, -1.000000000000000000 ) ) ;
#4161 = AXIS2_PLACEMENT_3D ( 'NONE', #3288, #2017, #5800 ) ;
#4162 = VERTEX_POINT ( 'NONE', #3172 ) ;
#4163 = DIRECTION ( 'NONE',  ( -0.000000000000000000, 1.000000000000000000, 1.224646799147353207E-16 ) ) ;
#4164 = EDGE_CURVE ( 'NONE', #3309, #4162, #7111, .T. ) ;
#4165 = FACE_OUTER_BOUND ( 'NONE', #473, .T. ) ;
#4166 = DIRECTION ( 'NONE',  ( 9.992007221626408864E-16, 1.000000000000000000, 0.000000000000000000 ) ) ;
#4167 = FACE_OUTER_BOUND ( 'NONE', #1883, .T. ) ;
#4168 = CIRCLE ( 'NONE', #3357, 4.171999999999999709 ) ;
#4169 = EDGE_LOOP ( 'NONE', ( #5143, #3938, #5437, #899, #1684 ) ) ;
#4170 = ADVANCED_FACE ( 'NONE', ( #6349 ), #3053, .F. ) ;
#4171 = EDGE_LOOP ( 'NONE', ( #748, #1714, #5862, #2303 ) ) ;
#4172 = VERTEX_POINT ( 'NONE', #5078 ) ;
#4173 = LINE ( 'NONE', #8114, #4677 ) ;
#4174 = CARTESIAN_POINT ( 'NONE',  ( -114.9999999999999147, 115.0000000000000000, -28.00000000000002487 ) ) ;
#4175 = ORIENTED_EDGE ( 'NONE', *, *, #6765, .F. ) ;
#4176 = CARTESIAN_POINT ( 'NONE',  ( -7.288983341925909798, -49.46703930816845940, -2.336970728266630548 ) ) ;
#4177 = CIRCLE ( 'NONE', #3648, 12.49999999999999289 ) ;
#4178 = FACE_OUTER_BOUND ( 'NONE', #5643, .T. ) ;
#4179 = CARTESIAN_POINT ( 'NONE',  ( 125.0000000000000000, 125.0000000000000284, 70.00000000000000000 ) ) ;
#4180 = VERTEX_POINT ( 'NONE', #2072 ) ;
#4181 = FACE_OUTER_BOUND ( 'NONE', #6935, .T. ) ;
#4182 = VERTEX_POINT ( 'NONE', #7843 ) ;
#4183 = DIRECTION ( 'NONE',  ( 1.000000000000000000, 0.000000000000000000, 0.000000000000000000 ) ) ;
#4184 = DIRECTION ( 'NONE',  ( 1.000000000000000000, 0.000000000000000000, 0.000000000000000000 ) ) ;
#4185 = ORIENTED_EDGE ( 'NONE', *, *, #922, .T. ) ;
#4186 = DIRECTION ( 'NONE',  ( -1.000000000000000000, 0.000000000000000000, 0.000000000000000000 ) ) ;
#4187 = DIRECTION ( 'NONE',  ( -0.000000000000000000, -0.000000000000000000, -1.000000000000000000 ) ) ;
#4188 = AXIS2_PLACEMENT_3D ( 'NONE', #5402, #7979, #7266 ) ;
#4189 = ORIENTED_EDGE ( 'NONE', *, *, #7897, .F. ) ;
#4190 = DIRECTION ( 'NONE',  ( 1.000000000000000000, 0.000000000000000000, 0.000000000000000000 ) ) ;
#4191 = ORIENTED_EDGE ( 'NONE', *, *, #7217, .F. ) ;
#4192 = EDGE_CURVE ( 'NONE', #5586, #3125, #3216, .T. ) ;
#4193 = CARTESIAN_POINT ( 'NONE',  ( 110.0000000000000142, -115.0000000000000000, 270.0000000000000000 ) ) ;
#4194 = DIRECTION ( 'NONE',  ( 0.000000000000000000, 0.000000000000000000, 1.000000000000000000 ) ) ;
#4195 = ORIENTED_EDGE ( 'NONE', *, *, #4419, .F. ) ;
#4196 = DIRECTION ( 'NONE',  ( -0.000000000000000000, 0.000000000000000000, 1.000000000000000000 ) ) ;
#4197 = CIRCLE ( 'NONE', #987, 12.50000000000000000 ) ;
#4198 = PRODUCT_DEFINITION_FORMATION_WITH_SPECIFIED_SOURCE ( 'ANY', '', #5128, .NOT_KNOWN. ) ;
#4199 = CARTESIAN_POINT ( 'NONE',  ( 125.0000000000000000, 125.0000000000000284, 0.000000000000000000 ) ) ;
#4200 = DIRECTION ( 'NONE',  ( 0.000000000000000000, 0.000000000000000000, 1.000000000000000000 ) ) ;
#4201 = ADVANCED_FACE ( 'NONE', ( #6515, #2025 ), #4568, .T. ) ;
#4202 = FACE_OUTER_BOUND ( 'NONE', #2954, .T. ) ;
#4203 = VECTOR ( 'NONE', #2740, 1000.000000000000000 ) ;
#4204 = EDGE_CURVE ( 'NONE', #5510, #5315, #741, .T. ) ;
#4205 = ORIENTED_EDGE ( 'NONE', *, *, #6855, .F. ) ;
#4206 = VERTEX_POINT ( 'NONE', #2561 ) ;
#4207 = ORIENTED_EDGE ( 'NONE', *, *, #735, .T. ) ;
#4208 = AXIS2_PLACEMENT_3D ( 'NONE', #5026, #1885, #1838 ) ;
#4209 = VERTEX_POINT ( 'NONE', #5881 ) ;
#4210 = DIRECTION ( 'NONE',  ( 1.000000000000000000, 0.000000000000000000, 0.000000000000000000 ) ) ;
#4211 = EDGE_CURVE ( 'NONE', #2952, #3213, #1982, .T. ) ;
#4212 = CARTESIAN_POINT ( 'NONE',  ( 10.00000000000000000, -3.448762466456902719E-14, 93.74999999999998579 ) ) ;
#4213 = EDGE_LOOP ( 'NONE', ( #6298, #5805 ) ) ;
#4214 = FILL_AREA_STYLE ('',( #2914 ) ) ;
#4215 = ORIENTED_EDGE ( 'NONE', *, *, #198, .F. ) ;
#4216 = CARTESIAN_POINT ( 'NONE',  ( 0.000000000000000000, -2.342598717236909600, -4.057499999999997442 ) ) ;
#4217 =( REPRESENTATION_RELATIONSHIP ('NONE','NONE', #6882, #2264 ) REPRESENTATION_RELATIONSHIP_WITH_TRANSFORMATION ( #3660 )SHAPE_REPRESENTATION_RELATIONSHIP( ) );
#4218 = DIRECTION ( 'NONE',  ( 1.000000000000000000, 0.000000000000000000, 0.000000000000000000 ) ) ;
#4219 = ORIENTED_EDGE ( 'NONE', *, *, #5928, .F. ) ;
#4220 = DIRECTION ( 'NONE',  ( 1.000000000000000000, 0.000000000000000000, 0.000000000000000000 ) ) ;
#4221 = EDGE_LOOP ( 'NONE', ( #1396, #1096, #4705, #4279, #4585 ) ) ;
#4222 = FACE_OUTER_BOUND ( 'NONE', #4694, .T. ) ;
#4223 = CYLINDRICAL_SURFACE ( 'NONE', #8037, 5.999999999999991118 ) ;
#4224 = LINE ( 'NONE', #7465, #7210 ) ;
#4225 = FACE_OUTER_BOUND ( 'NONE', #4608, .T. ) ;
#4226 =( GEOMETRIC_REPRESENTATION_CONTEXT ( 3 ) GLOBAL_UNCERTAINTY_ASSIGNED_CONTEXT ( ( #2850 ) ) GLOBAL_UNIT_ASSIGNED_CONTEXT ( ( #2311, #5131, #3720 ) ) REPRESENTATION_CONTEXT ( 'NONE', 'WORKASPACE' ) );
#4227 = ORIENTED_EDGE ( 'NONE', *, *, #6450, .F. ) ;
#4228 = DIRECTION ( 'NONE',  ( 0.000000000000000000, 0.4999999999999984457, -0.8660254037844394848 ) ) ;
#4229 = ORIENTED_EDGE ( 'NONE', *, *, #4058, .F. ) ;
#4230 = CARTESIAN_POINT ( 'NONE',  ( 5.000000000000000000, 7.027796151710712813, -4.057500000000006324 ) ) ;
#4231 = B_SPLINE_CURVE_WITH_KNOTS ( 'NONE', 3,
 ( #3001, #1627, #5592, #2350, #993, #4252, #8117, #4944, #1077, #4176, #3679, #341, #2391, #3582, #6256, #3539, #6119, #8168, #3631, #6169, #479, #2310, #7455, #5419, #7996, #7494, #2236, #1707, #7365, #4775, #1582, #3095, #3131, #1890, #5756, #4432, #3726, #1975, #3046, #3776, #7717, #5162, #6381, #4387, #522, #5678, #4993, #2598, #1798, #6346 ),
 .UNSPECIFIED., .F., .F.,
 ( 4, 2, 2, 2, 2, 2, 2, 2, 2, 2, 2, 2, 2, 2, 2, 2, 2, 2, 2, 2, 2, 2, 2, 2, 4 ),
 ( 0.000000000000000000, 0.002452303327911183745, 0.003678454991866776051, 0.004904606655822365754, 0.007356909983733550366, 0.008583061647689143106, 0.009809213311644733244, 0.01226151663955592046, 0.01348766830351151406, 0.01471381996746710594, 0.01593997163142269607, 0.01716612329537828968, 0.01961842662328948036, 0.02207072995120067452, 0.02452303327911185826, 0.02574918494306745534, 0.02697533660702304548, 0.02820148827097863561, 0.02942763993493422922, 0.03187994326284540603, 0.03310609492680098576, 0.03433224659075657242, 0.03678454991866773882, 0.03801070158262331855, 0.03923685324657889828 ),
 .UNSPECIFIED. ) ;
#4232 = EDGE_LOOP ( 'NONE', ( #4915, #5130, #8227, #169, #1852 ) ) ;
#4233 = APPLICATION_PROTOCOL_DEFINITION ( 'draft international standard', 'automotive_design', 1998, #77 ) ;
#4234 = ORIENTED_EDGE ( 'NONE', *, *, #5263, .F. ) ;
#4235 = CARTESIAN_POINT ( 'NONE',  ( 7.288983341925910686, 49.46703930816845940, -2.336970728266630992 ) ) ;
#4236 = VECTOR ( 'NONE', #2754, 1000.000000000000000 ) ;
#4237 = ADVANCED_FACE ( 'NONE', ( #2641 ), #655, .T. ) ;
#4238 = VECTOR ( 'NONE', #7804, 1000.000000000000000 ) ;
#4239 = ORIENTED_EDGE ( 'NONE', *, *, #2141, .F. ) ;
#4240 = CARTESIAN_POINT ( 'NONE',  ( -120.4999999999999716, 114.9999999999999858, 10.00000000000000000 ) ) ;
#4241 = DIRECTION ( 'NONE',  ( -0.000000000000000000, -0.000000000000000000, 1.000000000000000000 ) ) ;
#4242 = CARTESIAN_POINT ( 'NONE',  ( 115.0000000000000000, 114.9999999999999716, 20.00000000000000000 ) ) ;
#4243 = VECTOR ( 'NONE', #1282, 1000.000000000000227 ) ;
#4244 = ORIENTED_EDGE ( 'NONE', *, *, #7362, .T. ) ;
#4245 = VERTEX_POINT ( 'NONE', #3820 ) ;
#4246 = ADVANCED_FACE ( 'NONE', ( #5123 ), #5209, .T. ) ;
#4247 = EDGE_CURVE ( 'NONE', #4245, #8175, #86, .T. ) ;
#4248 = VECTOR ( 'NONE', #7064, 1000.000000000000000 ) ;
#4249 = LINE ( 'NONE', #5628, #2620 ) ;
#4250 = CARTESIAN_POINT ( 'NONE',  ( -49.00000000000000000, 55.00000000000000711, 27.50000000000000000 ) ) ;
#4251 = CARTESIAN_POINT ( 'NONE',  ( -10.00000000000000000, -3.448762466456902719E-14, 93.74999999999998579 ) ) ;
#4252 = CARTESIAN_POINT ( 'NONE',  ( -4.030269011847451566, -49.83886670901035387, -0.6603997896886458774 ) ) ;
#4253 = VECTOR ( 'NONE', #4778, 1000.000000000000000 ) ;
#4254 = EDGE_CURVE ( 'NONE', #2918, #7952, #1215, .T. ) ;
#4255 = ORIENTED_EDGE ( 'NONE', *, *, #76, .T. ) ;
#4256 = DIRECTION ( 'NONE',  ( 1.000000000000000000, 0.000000000000000000, 0.000000000000000000 ) ) ;
#4257 = VECTOR ( 'NONE', #2511, 1000.000000000000000 ) ;
#4258 = DIRECTION ( 'NONE',  ( 1.000000000000000000, 0.000000000000000000, 0.000000000000000000 ) ) ;
#4259 = ORIENTED_EDGE ( 'NONE', *, *, #5406, .F. ) ;
#4260 = VECTOR ( 'NONE', #5978, 1000.000000000000000 ) ;
#4261 = ORIENTED_EDGE ( 'NONE', *, *, #3024, .F. ) ;
#4262 = CARTESIAN_POINT ( 'NONE',  ( -10.00000000000000000, -55.00000000000000711, 93.74999999999998579 ) ) ;
#4263 = CARTESIAN_POINT ( 'NONE',  ( 4.038684223623524083, -49.84236097863851711, -24.35762614583959618 ) ) ;
#4264 = AXIS2_PLACEMENT_3D ( 'NONE', #4157, #2852, #7386 ) ;
#4265 = FACE_BOUND ( 'NONE', #2973, .T. ) ;
#4266 = EDGE_CURVE ( 'NONE', #6775, #6896, #6977, .T. ) ;
#4267 = SHAPE_REPRESENTATION ( 'Timing belt', ( #1299 ), #2092 ) ;
#4268 = ORIENTED_EDGE ( 'NONE', *, *, #4523, .F. ) ;
#4269 = ORIENTED_EDGE ( 'NONE', *, *, #2815, .F. ) ;
#4270 = ORIENTED_EDGE ( 'NONE', *, *, #7626, .T. ) ;
#4271 = CARTESIAN_POINT ( 'NONE',  ( 106.0000000000000142, 114.9999999999999716, 10.00000000000000000 ) ) ;
#4272 = AXIS2_PLACEMENT_3D ( 'NONE', #4843, #3657, #3607 ) ;
#4273 = DIRECTION ( 'NONE',  ( 1.000000000000000000, 0.000000000000000000, 0.000000000000000000 ) ) ;
#4274 = AXIS2_PLACEMENT_3D ( 'NONE', #3383, #2690, #5973 ) ;
#4275 = EDGE_LOOP ( 'NONE', ( #7611, #2689, #6241 ) ) ;
#4276 = DIRECTION ( 'NONE',  ( 0.000000000000000000, 0.000000000000000000, -1.000000000000000000 ) ) ;
#4277 = LINE ( 'NONE', #5011, #2698 ) ;
#4278 = LINE ( 'NONE', #3750, #2659 ) ;
#4279 = ORIENTED_EDGE ( 'NONE', *, *, #5716, .F. ) ;
#4280 = PRODUCT_CONTEXT ( 'NONE', #8297, 'mechanical' ) ;
#4281 = ORIENTED_EDGE ( 'NONE', *, *, #7807, .T. ) ;
#4282 = LINE ( 'NONE', #6880, #7706 ) ;
#4283 = VECTOR ( 'NONE', #6739, 1000.000000000000000 ) ;
#4284 = PLANE ( 'NONE',  #3068 ) ;
#4285 = ORIENTED_EDGE ( 'NONE', *, *, #5406, .T. ) ;
#4286 = CARTESIAN_POINT ( 'NONE',  ( 114.9999999999999147, 115.0000000000000000, 0.000000000000000000 ) ) ;
#4287 = AXIS2_PLACEMENT_3D ( 'NONE', #4943, #2514, #6297 ) ;
#4288 = DIRECTION ( 'NONE',  ( -0.000000000000000000, -0.000000000000000000, -1.000000000000000000 ) ) ;
#4289 = VECTOR ( 'NONE', #2055, 1000.000000000000000 ) ;
#4290 = ORIENTED_EDGE ( 'NONE', *, *, #7429, .T. ) ;
#4291 = LINE ( 'NONE', #1068, #5903 ) ;
#4292 = ORIENTED_EDGE ( 'NONE', *, *, #1907, .T. ) ;
#4293 = CARTESIAN_POINT ( 'NONE',  ( 55.00000000000000000, 55.00000000000000000, 220.0000000000000284 ) ) ;
#4294 = VECTOR ( 'NONE', #2138, 1000.000000000000000 ) ;
#4295 = CARTESIAN_POINT ( 'NONE',  ( 0.000000000000000000, -125.0000000000000000, -25.00000000000000000 ) ) ;
#4296 = EDGE_CURVE ( 'NONE', #5826, #3864, #4696, .T. ) ;
#4297 = PRODUCT ( 'Probe head motor', 'Probe head motor', '', ( #4280 ) ) ;
#4298 = CARTESIAN_POINT ( 'NONE',  ( 75.00000000000000000, -75.00000000000000000, 27.50000000000000000 ) ) ;
#4299 = EDGE_CURVE ( 'NONE', #4717, #110, #7112, .T. ) ;
#4300 = ORIENTED_EDGE ( 'NONE', *, *, #7602, .T. ) ;
#4301 = CARTESIAN_POINT ( 'NONE',  ( -115.0000000000000000, 115.0000000000000000, 20.00000000000000355 ) ) ;
#4302 = VERTEX_POINT ( 'NONE', #1579 ) ;
#4303 = EDGE_LOOP ( 'NONE', ( #4883, #3609 ) ) ;
#4304 = DIRECTION ( 'NONE',  ( 1.000000000000000000, 0.000000000000000000, 0.000000000000000000 ) ) ;
#4305 = LINE ( 'NONE', #2015, #5109 ) ;
#4306 = CYLINDRICAL_SURFACE ( 'NONE', #4493, 5.000000000000004441 ) ;
#4307 = ORIENTED_EDGE ( 'NONE', *, *, #3223, .F. ) ;
#4308 = CYLINDRICAL_SURFACE ( 'NONE', #6865, 5.000000000000035527 ) ;
#4309 = ADVANCED_FACE ( 'NONE', ( #7993 ), #2232, .T. ) ;
#4310 = ADVANCED_FACE ( 'NONE', ( #5373 ), #4089, .T. ) ;
#4311 = CYLINDRICAL_SURFACE ( 'NONE', #3324, 20.00000000000000355 ) ;
#4312 = ORIENTED_EDGE ( 'NONE', *, *, #5355, .F. ) ;
#4313 = CARTESIAN_POINT ( 'NONE',  ( -114.9999999999999147, -100.0000000000000000, 250.0000000000000000 ) ) ;
#4314 = VERTEX_POINT ( 'NONE', #1455 ) ;
#4315 = EDGE_LOOP ( 'NONE', ( #2713, #1032, #2461, #6410 ) ) ;
#4316 = DIRECTION ( 'NONE',  ( -1.000000000000000000, -0.000000000000000000, -0.000000000000000000 ) ) ;
#4317 = DIRECTION ( 'NONE',  ( 0.000000000000000000, -1.000000000000000000, 1.586032892321652236E-16 ) ) ;
#4318 = DIRECTION ( 'NONE',  ( -0.000000000000000000, -0.000000000000000000, 1.000000000000000000 ) ) ;
#4319 = ORIENTED_EDGE ( 'NONE', *, *, #1248, .T. ) ;
#4320 = FACE_OUTER_BOUND ( 'NONE', #6679, .T. ) ;
#4321 = EDGE_CURVE ( 'NONE', #1665, #5271, #3059, .T. ) ;
#4322 = ADVANCED_FACE ( 'NONE', ( #903, #4053 ), #297, .F. ) ;
#4323 = CYLINDRICAL_SURFACE ( 'NONE', #5394, 8.000000000000000000 ) ;
#4324 = PRODUCT_CONTEXT ( 'NONE', #7154, 'mechanical' ) ;
#4325 = ORIENTED_EDGE ( 'NONE', *, *, #6182, .T. ) ;
#4326 = CARTESIAN_POINT ( 'NONE',  ( 109.0000000000000426, -115.0000000000000000, 70.00000000000000000 ) ) ;
#4327 = CARTESIAN_POINT ( 'NONE',  ( 79.17200000000011073, 0.000000000000000000, 0.000000000000000000 ) ) ;
#4328 = CIRCLE ( 'NONE', #4188, 5.999999999999991118 ) ;
#4329 = VERTEX_POINT ( 'NONE', #3407 ) ;
#4330 = LINE ( 'NONE', #3615, #3200 ) ;
#4331 = DIRECTION ( 'NONE',  ( 0.000000000000000000, 0.8660254037844380415, -0.5000000000000011102 ) ) ;
#4332 = DIRECTION ( 'NONE',  ( -0.000000000000000000, 1.295896757998781966E-15, 1.000000000000000000 ) ) ;
#4333 = ORIENTED_EDGE ( 'NONE', *, *, #2865, .T. ) ;
#4334 = DIRECTION ( 'NONE',  ( 0.000000000000000000, 1.000000000000000000, -1.295896757998781966E-15 ) ) ;
#4335 = ORIENTED_EDGE ( 'NONE', *, *, #8225, .T. ) ;
#4336 = LINE ( 'NONE', #7749, #7800 ) ;
#4337 = ORIENTED_EDGE ( 'NONE', *, *, #5620, .T. ) ;
#4338 = CARTESIAN_POINT ( 'NONE',  ( -10.00000000000000000, -57.99999999999995737, -93.75000000000001421 ) ) ;
#4339 = LINE ( 'NONE', #3090, #2272 ) ;
#4340 = ITEM_DEFINED_TRANSFORMATION ( 'NONE', 'NONE', #4884,  #1299 ) ;
#4341 = LINE ( 'NONE', #4298, #6735 ) ;
#4342 = ORIENTED_EDGE ( 'NONE', *, *, #6688, .T. ) ;
#4343 = CARTESIAN_POINT ( 'NONE',  ( 0.000000000000000000, 125.0000000000000568, 79.99999999999992895 ) ) ;
#4344 = DIRECTION ( 'NONE',  ( -0.1584884973581717482, 9.126014887601318403E-17, -0.9873608237139798183 ) ) ;
#4345 = LINE ( 'NONE', #333, #7920 ) ;
#4346 = ORIENTED_EDGE ( 'NONE', *, *, #5085, .F. ) ;
#4347 = DIRECTION ( 'NONE',  ( 0.000000000000000000, 1.000000000000000000, 0.000000000000000000 ) ) ;
#4348 = EDGE_CURVE ( 'NONE', #877, #8314, #3584, .T. ) ;
#4349 = CARTESIAN_POINT ( 'NONE',  ( 5.000000000000000000, 2.342598717236902939, -4.057500000000001883 ) ) ;
#4350 = DIRECTION ( 'NONE',  ( -0.000000000000000000, -0.000000000000000000, 1.000000000000000000 ) ) ;
#4351 = CARTESIAN_POINT ( 'NONE',  ( 95.00000000000002842, -95.00000000000002842, 35.00000000000000000 ) ) ;
#4352 = CARTESIAN_POINT ( 'NONE',  ( 12.17681684015966503, -48.49465898589868118, -15.35333092327343785 ) ) ;
#4353 = ADVANCED_FACE ( 'NONE', ( #1502 ), #7915, .T. ) ;
#4354 = FACE_OUTER_BOUND ( 'NONE', #2071, .T. ) ;
#4355 = AXIS2_PLACEMENT_3D ( 'NONE', #4570, #3619, #3337 ) ;
#4356 = ORIENTED_EDGE ( 'NONE', *, *, #3533, .T. ) ;
#4357 = ADVANCED_FACE ( 'NONE', ( #6641 ), #2870, .F. ) ;
#4358 = EDGE_CURVE ( 'NONE', #4855, #1427, #4770, .T. ) ;
#4359 = UNCERTAINTY_MEASURE_WITH_UNIT (LENGTH_MEASURE( 1.000000000000000082E-05 ), #3691, 'distance_accuracy_value', 'NONE');
#4360 = ORIENTED_EDGE ( 'NONE', *, *, #2632, .T. ) ;
#4361 = CARTESIAN_POINT ( 'NONE',  ( -59.99999999999999289, 55.00000000000000000, 220.0000000000000284 ) ) ;
#4362 = FACE_OUTER_BOUND ( 'NONE', #4998, .T. ) ;
#4363 = DIRECTION ( 'NONE',  ( -1.000000000000000000, -0.000000000000000000, -0.000000000000000000 ) ) ;
#4364 = VECTOR ( 'NONE', #4059, 1000.000000000000000 ) ;
#4365 = EDGE_LOOP ( 'NONE', ( #4926, #6002, #6830, #1773 ) ) ;
#4366 = CARTESIAN_POINT ( 'NONE',  ( 10.00000000000000000, -3.448762466456902719E-14, 151.7499999999999432 ) ) ;
#4367 = CYLINDRICAL_SURFACE ( 'NONE', #627, 8.999999999999994671 ) ;
#4368 = SHAPE_DEFINITION_REPRESENTATION ( #8091, #239 ) ;
#4369 = ORIENTED_EDGE ( 'NONE', *, *, #6489, .F. ) ;
#4370 = CARTESIAN_POINT ( 'NONE',  ( 0.000000000000000000, 0.000000000000000000, 15.00000000000000000 ) ) ;
#4371 = DIRECTION ( 'NONE',  ( 1.000000000000000000, 0.000000000000000000, 0.000000000000000000 ) ) ;
#4372 = ADVANCED_FACE ( 'NONE', ( #2793, #5298 ), #7880, .T. ) ;
#4373 = ORIENTED_EDGE ( 'NONE', *, *, #5064, .F. ) ;
#4374 = CARTESIAN_POINT ( 'NONE',  ( 0.000000000000000000, 0.000000000000000000, 15.00000000000000000 ) ) ;
#4375 = VERTEX_POINT ( 'NONE', #7317 ) ;
#4376 = DIRECTION ( 'NONE',  ( 0.000000000000000000, -2.960594732333750117E-16, 1.000000000000000000 ) ) ;
#4377 = VERTEX_POINT ( 'NONE', #2110 ) ;
#4378 = CARTESIAN_POINT ( 'NONE',  ( -5.536947881659091131, 49.69381142126947992, -23.71430020744633183 ) ) ;
#4379 = VERTEX_POINT ( 'NONE', #5332 ) ;
#4380 = EDGE_LOOP ( 'NONE', ( #5714, #452, #5454 ) ) ;
#4381 = EDGE_CURVE ( 'NONE', #7564, #900, #8331, .T. ) ;
#4382 = DIRECTION ( 'NONE',  ( 0.000000000000000000, 1.000000000000000000, 0.000000000000000000 ) ) ;
#4383 = VECTOR ( 'NONE', #2746, 1000.000000000000000 ) ;
#4384 = VECTOR ( 'NONE', #2402, 1000.000000000000000 ) ;
#4385 = CARTESIAN_POINT ( 'NONE',  ( 105.0000000000000000, -105.0000000000000568, 20.00000000000001776 ) ) ;
#4386 = VERTEX_POINT ( 'NONE', #7233 ) ;
#4387 = CARTESIAN_POINT ( 'NONE',  ( -4.037232620646160619, -49.84250566375262537, -24.35825330067164174 ) ) ;
#4388 = AXIS2_PLACEMENT_3D ( 'NONE', #483, #1084, #1127 ) ;
#4389 = LINE ( 'NONE', #4349, #1578 ) ;
#4390 = CARTESIAN_POINT ( 'NONE',  ( -54.99999999999999289, -54.99999999999999289, 27.50000000000000000 ) ) ;
#4391 = CARTESIAN_POINT ( 'NONE',  ( 0.8292248493948921606, -50.00000000000000711, -9.486769009248113261E-17 ) ) ;
#4392 = DIRECTION ( 'NONE',  ( 0.000000000000000000, 1.000000000000000000, 0.000000000000000000 ) ) ;
#4393 = VECTOR ( 'NONE', #263, 1000.000000000000000 ) ;
#4394 = DIRECTION ( 'NONE',  ( 1.000000000000000000, 0.000000000000000000, 0.000000000000000000 ) ) ;
#4395 = ORIENTED_EDGE ( 'NONE', *, *, #1188, .T. ) ;
#4396 = AXIS2_PLACEMENT_3D ( 'NONE', #1972, #5956, #164 ) ;
#4397 = CARTESIAN_POINT ( 'NONE',  ( 4.592425496802573578E-15, -37.49999999999999289, -150.0000000000000000 ) ) ;
#4398 = EDGE_LOOP ( 'NONE', ( #1055, #1223 ) ) ;
#4399 = DIRECTION ( 'NONE',  ( -0.000000000000000000, -0.000000000000000000, 1.000000000000000000 ) ) ;
#4400 = ORIENTED_EDGE ( 'NONE', *, *, #5871, .T. ) ;
#4401 = CARTESIAN_POINT ( 'NONE',  ( 4.999999999999994671, -3.755786496842898268E-15, -4.057500000000000107 ) ) ;
#4402 = DIRECTION ( 'NONE',  ( 1.000000000000000000, 0.000000000000000000, 0.000000000000000000 ) ) ;
#4403 = CIRCLE ( 'NONE', #2545, 5.499999999999991118 ) ;
#4404 = ADVANCED_FACE ( 'NONE', ( #7193 ), #3994, .F. ) ;
#4405 = VERTEX_POINT ( 'NONE', #827 ) ;
#4406 = SHAPE_DEFINITION_REPRESENTATION ( #2064, #2264 ) ;
#4407 = ADVANCED_FACE ( 'NONE', ( #3371 ), #1159, .F. ) ;
#4408 = CIRCLE ( 'NONE', #5097, 5.999999999999991118 ) ;
#4409 = ORIENTED_EDGE ( 'NONE', *, *, #7798, .T. ) ;
#4410 = FACE_OUTER_BOUND ( 'NONE', #3718, .T. ) ;
#4411 = EDGE_LOOP ( 'NONE', ( #3728, #6727, #8018, #1452, #3032 ) ) ;
#4412 = AXIS2_PLACEMENT_3D ( 'NONE', #1668, #7417, #6086 ) ;
#4413 = VERTEX_POINT ( 'NONE', #6294 ) ;
#4414 = DIRECTION ( 'NONE',  ( -0.000000000000000000, -1.632680918566406547E-16, 1.000000000000000000 ) ) ;
#4415 = ORIENTED_EDGE ( 'NONE', *, *, #3089, .T. ) ;
#4416 = DIRECTION ( 'NONE',  ( -0.000000000000000000, -0.000000000000000000, 1.000000000000000000 ) ) ;
#4417 = EDGE_CURVE ( 'NONE', #6215, #3867, #1794, .T. ) ;
#4418 = EDGE_LOOP ( 'NONE', ( #4436, #4827, #2732, #6248 ) ) ;
#4419 = EDGE_CURVE ( 'NONE', #8288, #8056, #4339, .T. ) ;
#4420 = EDGE_CURVE ( 'NONE', #8051, #4528, #2538, .T. ) ;
#4421 = AXIS2_PLACEMENT_3D ( 'NONE', #174, #6645, #5846 ) ;
#4422 = CIRCLE ( 'NONE', #4982, 5.999999999999991118 ) ;
#4423 = CARTESIAN_POINT ( 'NONE',  ( -5.167842669270958034, 49.73365441721957581, -23.88900650468791298 ) ) ;
#4424 = CARTESIAN_POINT ( 'NONE',  ( -105.0000000000000000, -72.50000000000000000, 240.0000000000000284 ) ) ;
#4425 = FACE_OUTER_BOUND ( 'NONE', #5866, .T. ) ;
#4426 = CARTESIAN_POINT ( 'NONE',  ( 102.5000000000000000, 0.000000000000000000, 0.000000000000000000 ) ) ;
#4427 = AXIS2_PLACEMENT_3D ( 'NONE', #5170, #7763, #1983 ) ;
#4428 = AXIS2_PLACEMENT_3D ( 'NONE', #4242, #6842, #3617 ) ;
#4429 = CYLINDRICAL_SURFACE ( 'NONE', #5257, 95.00000000000001421 ) ;
#4430 = EDGE_LOOP ( 'NONE', ( #4097, #6291, #2611, #357 ) ) ;
#4431 = EDGE_CURVE ( 'NONE', #984, #431, #4173, .T. ) ;
#4432 = CARTESIAN_POINT ( 'NONE',  ( -9.403255565416666073, -49.10853579810842717, -20.74590799004609210 ) ) ;
#4433 = ADVANCED_FACE ( 'NONE', ( #8162 ), #2957, .F. ) ;
#4434 = DIRECTION ( 'NONE',  ( 0.000000000000000000, 0.000000000000000000, 1.000000000000000000 ) ) ;
#4435 = VECTOR ( 'NONE', #7754, 1000.000000000000114 ) ;
#4436 = ORIENTED_EDGE ( 'NONE', *, *, #1357, .F. ) ;
#4437 = EDGE_CURVE ( 'NONE', #1562, #2572, #3041, .T. ) ;
#4438 = DIRECTION ( 'NONE',  ( 0.000000000000000000, -0.4999999999999985012, 0.8660254037844393737 ) ) ;
#4439 = DIRECTION ( 'NONE',  ( 0.000000000000000000, 0.000000000000000000, 1.000000000000000000 ) ) ;
#4440 = CARTESIAN_POINT ( 'NONE',  ( 1.646459091894410642, -49.97939023862976882, -0.08171336424531111531 ) ) ;
#4441 = CARTESIAN_POINT ( 'NONE',  ( 121.0000000000000000, 115.0000000000000000, 20.00000000000000355 ) ) ;
#4442 = PRODUCT_DEFINITION_SHAPE ( 'NONE', 'NONE',  #8366 ) ;
#4443 = FACE_OUTER_BOUND ( 'NONE', #5398, .T. ) ;
#4444 = VERTEX_POINT ( 'NONE', #1071 ) ;
#4445 = ORIENTED_EDGE ( 'NONE', *, *, #5253, .T. ) ;
#4446 = UNCERTAINTY_MEASURE_WITH_UNIT (LENGTH_MEASURE( 1.000000000000000082E-05 ), #5803, 'distance_accuracy_value', 'NONE');
#4447 = ORIENTED_EDGE ( 'NONE', *, *, #680, .F. ) ;
#4448 = CARTESIAN_POINT ( 'NONE',  ( 121.0000000000000284, -115.0000000000000000, 70.00000000000000000 ) ) ;
#4449 = ORIENTED_EDGE ( 'NONE', *, *, #2130, .T. ) ;
#4450 = DIRECTION ( 'NONE',  ( 0.000000000000000000, 0.000000000000000000, 1.000000000000000000 ) ) ;
#4451 = FACE_OUTER_BOUND ( 'NONE', #1754, .T. ) ;
#4452 = CONTEXT_DEPENDENT_SHAPE_REPRESENTATION ( #3925, #8164 ) ;
#4453 = DIRECTION ( 'NONE',  ( 1.000000000000000000, 0.000000000000000000, 0.000000000000000000 ) ) ;
#4454 = AXIS2_PLACEMENT_3D ( 'NONE', #7895, #1391, #6532 ) ;
#4455 = ORIENTED_EDGE ( 'NONE', *, *, #6307, .T. ) ;
#4456 = DIRECTION ( 'NONE',  ( -0.000000000000000000, -0.000000000000000000, 1.000000000000000000 ) ) ;
#4457 = ORIENTED_EDGE ( 'NONE', *, *, #5281, .T. ) ;
#4458 = ADVANCED_FACE ( 'NONE', ( #3534 ), #2909, .F. ) ;
#4459 = FACE_OUTER_BOUND ( 'NONE', #3671, .T. ) ;
#4460 = ADVANCED_FACE ( 'NONE', ( #6163 ), #429, .T. ) ;
#4461 = ORIENTED_EDGE ( 'NONE', *, *, #2866, .T. ) ;
#4462 = CARTESIAN_POINT ( 'NONE',  ( 50.00000000000000000, -55.00000000000000000, 240.0000000000000284 ) ) ;
#4463 = DIRECTION ( 'NONE',  ( 6.106226635438361958E-16, 0.000000000000000000, 1.000000000000000000 ) ) ;
#4464 = ORIENTED_EDGE ( 'NONE', *, *, #1759, .F. ) ;
#4465 = DIRECTION ( 'NONE',  ( 0.000000000000000000, 0.000000000000000000, -1.000000000000000000 ) ) ;
#4466 = CARTESIAN_POINT ( 'NONE',  ( -7.631816331990290081, 49.41886753685898270, -22.43335506184081751 ) ) ;
#4467 = AXIS2_PLACEMENT_3D ( 'NONE', #6068, #282, #5445 ) ;
#4468 = DIRECTION ( 'NONE',  ( -0.000000000000000000, -0.000000000000000000, 1.000000000000000000 ) ) ;
#4469 = ADVANCED_FACE ( 'NONE', ( #475 ), #4941, .T. ) ;
#4470 = CARTESIAN_POINT ( 'NONE',  ( 120.9999999999999005, -115.0000000000000000, -28.00000000000002487 ) ) ;
#4471 = CARTESIAN_POINT ( 'NONE',  ( 0.000000000000000000, 125.0000000000000568, 66.99999999999992895 ) ) ;
#4472 = VECTOR ( 'NONE', #6027, 1000.000000000000000 ) ;
#4473 = FACE_OUTER_BOUND ( 'NONE', #7698, .T. ) ;
#4474 = ORIENTED_EDGE ( 'NONE', *, *, #4685, .T. ) ;
#4475 = CARTESIAN_POINT ( 'NONE',  ( 55.00000000000000000, -55.00000000000000000, 220.0000000000000284 ) ) ;
#4476 = ORIENTED_EDGE ( 'NONE', *, *, #1867, .F. ) ;
#4477 = DIRECTION ( 'NONE',  ( -0.000000000000000000, -0.000000000000000000, 1.000000000000000000 ) ) ;
#4478 = CARTESIAN_POINT ( 'NONE',  ( -120.4999999999999716, 114.9999999999999858, 0.000000000000000000 ) ) ;
#4479 = DIRECTION ( 'NONE',  ( -0.000000000000000000, 1.000000000000000000, 1.266875999117951024E-16 ) ) ;
#4480 = CLOSED_SHELL ( 'NONE', ( #3035, #1752, #2398, #3372, #97, #5773 ) ) ;
#4481 = CARTESIAN_POINT ( 'NONE',  ( 10.84023063519268071, -48.81293515762428115, -18.77686690299335481 ) ) ;
#4482 = CARTESIAN_POINT ( 'NONE',  ( -49.00000000000000000, -55.00000000000000711, 27.50000000000000000 ) ) ;
#4483 = LINE ( 'NONE', #7073, #7893 ) ;
#4484 = CYLINDRICAL_SURFACE ( 'NONE', #3195, 12.99999999999999822 ) ;
#4485 = VERTEX_POINT ( 'NONE', #5588 ) ;
#4486 = VERTEX_POINT ( 'NONE', #4295 ) ;
#4487 = ORIENTED_EDGE ( 'NONE', *, *, #2925, .T. ) ;
#4488 = CARTESIAN_POINT ( 'NONE',  ( -10.00000000000000000, 54.99999999999989342, 93.75000000000004263 ) ) ;
#4489 = ORIENTED_EDGE ( 'NONE', *, *, #5623, .T. ) ;
#4490 = CARTESIAN_POINT ( 'NONE',  ( 114.9999999999999858, -115.0000000000000000, 266.9956969048622568 ) ) ;
#4491 = CARTESIAN_POINT ( 'NONE',  ( 75.00000000000001421, 9.184850993605150311E-15, 15.00000000000000000 ) ) ;
#4492 = DIRECTION ( 'NONE',  ( -0.000000000000000000, -0.000000000000000000, 1.000000000000000000 ) ) ;
#4493 = AXIS2_PLACEMENT_3D ( 'NONE', #6906, #7588, #4220 ) ;
#4494 = VERTEX_POINT ( 'NONE', #6892 ) ;
#4495 = CARTESIAN_POINT ( 'NONE',  ( 9.403255565416678508, 49.10853579810846270, -20.74590799004608854 ) ) ;
#4496 = ORIENTED_EDGE ( 'NONE', *, *, #2866, .F. ) ;
#4497 = CARTESIAN_POINT ( 'NONE',  ( 75.00000000000000000, 0.000000000000000000, 0.000000000000000000 ) ) ;
#4498 = ORIENTED_EDGE ( 'NONE', *, *, #8299, .T. ) ;
#4499 =( REPRESENTATION_RELATIONSHIP ('NONE','NONE', #6882, #239 ) REPRESENTATION_RELATIONSHIP_WITH_TRANSFORMATION ( #2657 )SHAPE_REPRESENTATION_RELATIONSHIP( ) );
#4500 = SURFACE_STYLE_FILL_AREA ( #6453 ) ;
#4501 = EDGE_CURVE ( 'NONE', #110, #1626, #1117, .T. ) ;
#4502 = CARTESIAN_POINT ( 'NONE',  ( -0.8175244905105707449, 50.00000000000000711, -25.00000000000000355 ) ) ;
#4503 = CARTESIAN_POINT ( 'NONE',  ( 0.000000000000000000, 0.000000000000000000, 15.00000000000000000 ) ) ;
#4504 = DIRECTION ( 'NONE',  ( -0.000000000000000000, -0.000000000000000000, 1.000000000000000000 ) ) ;
#4505 = CARTESIAN_POINT ( 'NONE',  ( 124.0000000000000000, 114.9999999999999716, 20.00000000000000000 ) ) ;
#4506 = DIRECTION ( 'NONE',  ( -0.000000000000000000, -0.000000000000000000, 1.000000000000000000 ) ) ;
#4507 = CARTESIAN_POINT ( 'NONE',  ( 0.000000000000000000, 0.000000000000000000, -120.5000000000000284 ) ) ;
#4508 = LINE ( 'NONE', #2744, #7287 ) ;
#4509 = ORIENTED_EDGE ( 'NONE', *, *, #5929, .T. ) ;
#4510 = DIRECTION ( 'NONE',  ( -0.9997971424738624213, 3.882625124175935815E-16, 0.02014134804572967688 ) ) ;
#4511 = ADVANCED_FACE ( 'NONE', ( #518 ), #3676, .F. ) ;
#4512 = EDGE_CURVE ( 'NONE', #2876, #210, #7406, .T. ) ;
#4513 = ADVANCED_FACE ( 'NONE', ( #1658 ), #1029, .F. ) ;
#4514 = ORIENTED_EDGE ( 'NONE', *, *, #5475, .F. ) ;
#4515 = ORIENTED_EDGE ( 'NONE', *, *, #6854, .T. ) ;
#4516 = AXIS2_PLACEMENT_3D ( 'NONE', #786, #7847, #4057 ) ;
#4517 = CARTESIAN_POINT ( 'NONE',  ( 115.0000000000000000, 115.0000000000000000, 20.00000000000000355 ) ) ;
#4518 = LINE ( 'NONE', #7152, #4639 ) ;
#4519 = DIRECTION ( 'NONE',  ( -0.000000000000000000, -0.000000000000000000, 1.000000000000000000 ) ) ;
#4520 = LINE ( 'NONE', #1336, #2564 ) ;
#4521 = DIRECTION ( 'NONE',  ( -0.000000000000000000, -0.000000000000000000, 1.000000000000000000 ) ) ;
#4522 = VECTOR ( 'NONE', #6832, 1000.000000000000000 ) ;
#4523 = EDGE_CURVE ( 'NONE', #3267, #326, #4900, .T. ) ;
#4524 = DIRECTION ( 'NONE',  ( 0.000000000000000000, 0.000000000000000000, -1.000000000000000000 ) ) ;
#4525 = ORIENTED_EDGE ( 'NONE', *, *, #4698, .T. ) ;
#4526 = DIRECTION ( 'NONE',  ( 0.000000000000000000, 0.000000000000000000, 1.000000000000000000 ) ) ;
#4527 = VECTOR ( 'NONE', #7067, 999.9999999999998863 ) ;
#4528 = VERTEX_POINT ( 'NONE', #4250 ) ;
#4529 = ORIENTED_EDGE ( 'NONE', *, *, #2865, .F. ) ;
#4530 = LINE ( 'NONE', #4707, #5913 ) ;
#4531 = EDGE_LOOP ( 'NONE', ( #6257, #6007, #1776, #1992 ) ) ;
#4532 = CARTESIAN_POINT ( 'NONE',  ( -115.0000000000000000, -115.0000000000000000, 270.0000000000000000 ) ) ;
#4533 = CARTESIAN_POINT ( 'NONE',  ( 9.999999999999998224, 0.000000000000000000, -5.400000000000035882 ) ) ;
#4534 = DIRECTION ( 'NONE',  ( 1.000000000000000000, 0.000000000000000000, 0.000000000000000000 ) ) ;
#4535 = ITEM_DEFINED_TRANSFORMATION ( 'NONE', 'NONE', #4068,  #1299 ) ;
#4536 = EDGE_CURVE ( 'NONE', #5024, #3768, #5230, .T. ) ;
#4537 = AXIS2_PLACEMENT_3D ( 'NONE', #2347, #3579, #5545 ) ;
#4538 = CARTESIAN_POINT ( 'NONE',  ( 55.00000000000000000, 55.00000000000000000, 240.0000000000000284 ) ) ;
#4539 = AXIS2_PLACEMENT_3D ( 'NONE', #5214, #2687, #5266 ) ;
#4540 = DIRECTION ( 'NONE',  ( -0.000000000000000000, 1.000000000000000000, 1.266875999117951024E-16 ) ) ;
#4541 = LINE ( 'NONE', #1917, #1733 ) ;
#4542 = ORIENTED_EDGE ( 'NONE', *, *, #4417, .F. ) ;
#4543 =( NAMED_UNIT ( * ) PLANE_ANGLE_UNIT ( ) SI_UNIT ( $, .RADIAN. ) );
#4544 = VECTOR ( 'NONE', #3011, 1000.000000000000000 ) ;
#4545 = CARTESIAN_POINT ( 'NONE',  ( 5.000000000000000000, -2.342598717236909600, -4.057499999999997442 ) ) ;
#4546 = CARTESIAN_POINT ( 'NONE',  ( -7.627277604624987717, 49.41585025822053012, -2.588352797709350561 ) ) ;
#4547 = AXIS2_PLACEMENT_3D ( 'NONE', #4979, #4331, #511 ) ;
#4548 = VECTOR ( 'NONE', #322, 1000.000000000000000 ) ;
#4549 = PLANE ( 'NONE',  #1254 ) ;
#4550 = AXIS2_PLACEMENT_3D ( 'NONE', #4038, #6625, #847 ) ;
#4551 = CYLINDRICAL_SURFACE ( 'NONE', #7474, 5.499999999999991118 ) ;
#4552 = DIRECTION ( 'NONE',  ( 0.000000000000000000, 1.000000000000000000, 0.000000000000000000 ) ) ;
#4553 = FACE_OUTER_BOUND ( 'NONE', #3463, .T. ) ;
#4554 = CIRCLE ( 'NONE', #1604, 4.999999999999990230 ) ;
#4555 = DIRECTION ( 'NONE',  ( -0.000000000000000000, -0.000000000000000000, 1.000000000000000000 ) ) ;
#4556 = VECTOR ( 'NONE', #999, 1000.000000000000000 ) ;
#4557 = LINE ( 'NONE', #81, #8085 ) ;
#4558 = EDGE_LOOP ( 'NONE', ( #6348, #4709, #3264, #3575, #7411 ) ) ;
#4559 = ORIENTED_EDGE ( 'NONE', *, *, #4321, .T. ) ;
#4560 = DIRECTION ( 'NONE',  ( -0.000000000000000000, -0.000000000000000000, -1.000000000000000000 ) ) ;
#4561 = DIRECTION ( 'NONE',  ( 0.9992060621654691444, -0.03984024763698791605, 1.223674505719567166E-16 ) ) ;
#4562 = ORIENTED_EDGE ( 'NONE', *, *, #8095, .T. ) ;
#4563 = EDGE_CURVE ( 'NONE', #6237, #1109, #6704, .T. ) ;
#4564 = AXIS2_PLACEMENT_3D ( 'NONE', #1088, #3643, #6222 ) ;
#4565 = AXIS2_PLACEMENT_3D ( 'NONE', #1323, #2634, #6463 ) ;
#4566 = ORIENTED_EDGE ( 'NONE', *, *, #7822, .T. ) ;
#4567 = FACE_OUTER_BOUND ( 'NONE', #2199, .T. ) ;
#4568 = PLANE ( 'NONE',  #3315 ) ;
#4569 = EDGE_CURVE ( 'NONE', #4494, #8125, #3845, .T. ) ;
#4570 = CARTESIAN_POINT ( 'NONE',  ( 0.000000000000000000, 4.500000000000000000, -128.0000000000000284 ) ) ;
#4571 = DIRECTION ( 'NONE',  ( 2.643388153869419325E-16, -1.000000000000000000, 0.000000000000000000 ) ) ;
#4572 =( LENGTH_UNIT ( ) NAMED_UNIT ( * ) SI_UNIT ( .MILLI., .METRE. ) );
#4573 = AXIS2_PLACEMENT_3D ( 'NONE', #2958, #5377, #5546 ) ;
#4574 = CIRCLE ( 'NONE', #2819, 12.50000000000000000 ) ;
#4575 = CARTESIAN_POINT ( 'NONE',  ( -75.00000000000001421, 0.000000000000000000, 35.00000000000000000 ) ) ;
#4576 = ORIENTED_EDGE ( 'NONE', *, *, #3415, .T. ) ;
#4577 = EDGE_CURVE ( 'NONE', #2109, #5395, #2666, .T. ) ;
#4578 = CARTESIAN_POINT ( 'NONE',  ( 124.9999999999997442, -125.0000000000000000, 20.00000000000000000 ) ) ;
#4579 = ORIENTED_EDGE ( 'NONE', *, *, #8053, .T. ) ;
#4580 = EDGE_CURVE ( 'NONE', #1935, #6702, #3810, .T. ) ;
#4581 = ORIENTED_EDGE ( 'NONE', *, *, #4956, .F. ) ;
#4582 = EDGE_CURVE ( 'NONE', #1706, #6062, #1190, .T. ) ;
#4583 = PLANE ( 'NONE',  #6991 ) ;
#4584 = ADVANCED_FACE ( 'NONE', ( #1839 ), #6504, .F. ) ;
#4585 = ORIENTED_EDGE ( 'NONE', *, *, #6489, .T. ) ;
#4586 = DIRECTION ( 'NONE',  ( -1.000000000000000000, -0.000000000000000000, -0.000000000000000000 ) ) ;
#4587 = CARTESIAN_POINT ( 'NONE',  ( 0.000000000000000000, 125.0000000000000568, 79.99999999999992895 ) ) ;
#4588 = ITEM_DEFINED_TRANSFORMATION ( 'NONE', 'NONE', #3137,  #1299 ) ;
#4589 = CARTESIAN_POINT ( 'NONE',  ( -109.0000000000000426, -115.0000000000000000, 70.00000000000000000 ) ) ;
#4590 = EDGE_LOOP ( 'NONE', ( #7012, #1644, #3124, #6368 ) ) ;
#4591 = PRODUCT_DEFINITION_SHAPE ( 'NONE', 'NONE',  #8364 ) ;
#4592 = CARTESIAN_POINT ( 'NONE',  ( -1.033895191682177028E-13, -12.50000000000001066, 12.50000000000000533 ) ) ;
#4593 = LINE ( 'NONE', #3355, #4960 ) ;
#4594 = ORIENTED_EDGE ( 'NONE', *, *, #735, .F. ) ;
#4595 = DIRECTION ( 'NONE',  ( 1.460819769243625652E-16, -1.000000000000000000, -0.000000000000000000 ) ) ;
#4596 = CIRCLE ( 'NONE', #3363, 8.999999999999994671 ) ;
#4597 = DIRECTION ( 'NONE',  ( -0.000000000000000000, -0.000000000000000000, 1.000000000000000000 ) ) ;
#4598 = CARTESIAN_POINT ( 'NONE',  ( 125.0000000000000000, 125.0000000000000000, 340.0000000000000000 ) ) ;
#4599 = LINE ( 'NONE', #6542, #2516 ) ;
#4600 = CARTESIAN_POINT ( 'NONE',  ( 0.000000000000000000, 1.986334338364416506E-15, 0.000000000000000000 ) ) ;
#4601 = CARTESIAN_POINT ( 'NONE',  ( 17.61817604250836311, -4.500000000000000000, -128.0000120000000265 ) ) ;
#4602 = DIRECTION ( 'NONE',  ( -0.000000000000000000, -1.000000000000000000, -0.000000000000000000 ) ) ;
#4603 = CYLINDRICAL_SURFACE ( 'NONE', #3215, 4.999999999999997335 ) ;
#4604 = DIRECTION ( 'NONE',  ( -0.000000000000000000, -0.000000000000000000, 1.000000000000000000 ) ) ;
#4605 = ORIENTED_EDGE ( 'NONE', *, *, #5514, .T. ) ;
#4606 = DIRECTION ( 'NONE',  ( -0.000000000000000000, 0.000000000000000000, 1.000000000000000000 ) ) ;
#4607 = DIRECTION ( 'NONE',  ( 1.000000000000000000, 3.155443620884047222E-30, 1.224646799147346798E-16 ) ) ;
#4608 = EDGE_LOOP ( 'NONE', ( #7923, #1552, #6054, #5606 ) ) ;
#4609 = CIRCLE ( 'NONE', #2085, 95.00000000000008527 ) ;
#4610 = DIRECTION ( 'NONE',  ( 1.000000000000000000, 0.000000000000000000, 0.000000000000000000 ) ) ;
#4611 = CARTESIAN_POINT ( 'NONE',  ( 120.0000000000000000, 125.0000000000000000, 0.000000000000000000 ) ) ;
#4612 = PLANE ( 'NONE',  #6188 ) ;
#4613 = PLANE ( 'NONE',  #753 ) ;
#4614 =( NAMED_UNIT ( * ) SI_UNIT ( $, .STERADIAN. ) SOLID_ANGLE_UNIT ( ) );
#4615 = AXIS2_PLACEMENT_3D ( 'NONE', #8081, #394, #2313 ) ;
#4616 = DIRECTION ( 'NONE',  ( 0.000000000000000000, 2.960594732333750610E-16, -1.000000000000000000 ) ) ;
#4617 = DIRECTION ( 'NONE',  ( -0.000000000000000000, -0.000000000000000000, -1.000000000000000000 ) ) ;
#4618 = CARTESIAN_POINT ( 'NONE',  ( 0.000000000000000000, 0.000000000000000000, -248.3416876048222832 ) ) ;
#4619 = ADVANCED_FACE ( 'NONE', ( #1203 ), #7142, .T. ) ;
#4620 = EDGE_LOOP ( 'NONE', ( #392, #7089 ) ) ;
#4621 = PLANE ( 'NONE',  #577 ) ;
#4622 =( REPRESENTATION_RELATIONSHIP ('NONE','NONE', #6882, #3965 ) REPRESENTATION_RELATIONSHIP_WITH_TRANSFORMATION ( #6146 )SHAPE_REPRESENTATION_RELATIONSHIP( ) );
#4623 = CIRCLE ( 'NONE', #1530, 54.99999999999996447 ) ;
#4624 = ORIENTED_EDGE ( 'NONE', *, *, #2348, .T. ) ;
#4625 = DIRECTION ( 'NONE',  ( 1.000000000000000000, 0.000000000000000000, 0.000000000000000000 ) ) ;
#4626 = ORIENTED_EDGE ( 'NONE', *, *, #5261, .F. ) ;
#4627 = FACE_OUTER_BOUND ( 'NONE', #962, .T. ) ;
#4628 = DIRECTION ( 'NONE',  ( 1.000000000000000000, 0.000000000000000000, 0.000000000000000000 ) ) ;
#4629 = CONTEXT_DEPENDENT_SHAPE_REPRESENTATION ( #6945, #692 ) ;
#4630 = CARTESIAN_POINT ( 'NONE',  ( 1.000000000000000888, 0.000000000000000000, 0.000000000000000000 ) ) ;
#4631 = EDGE_CURVE ( 'NONE', #3543, #4652, #5751, .T. ) ;
#4632 = AXIS2_PLACEMENT_3D ( 'NONE', #2549, #1070, #728 ) ;
#4633 = EDGE_CURVE ( 'NONE', #1402, #6246, #644, .T. ) ;
#4634 = EDGE_LOOP ( 'NONE', ( #2182, #7769, #1195, #2991 ) ) ;
#4635 = LINE ( 'NONE', #2583, #3152 ) ;
#4636 = DIRECTION ( 'NONE',  ( -0.000000000000000000, -0.000000000000000000, -1.000000000000000000 ) ) ;
#4637 = ORIENTED_EDGE ( 'NONE', *, *, #8257, .F. ) ;
#4638 =( LENGTH_UNIT ( ) NAMED_UNIT ( * ) SI_UNIT ( .MILLI., .METRE. ) );
#4639 = VECTOR ( 'NONE', #5963, 1000.000000000000000 ) ;
#4640 = ORIENTED_EDGE ( 'NONE', *, *, #830, .T. ) ;
#4641 = CARTESIAN_POINT ( 'NONE',  ( -1.646459091894399984, 49.97939023862978303, -0.08171336424531015774 ) ) ;
#4642 = EDGE_CURVE ( 'NONE', #3406, #8276, #3207, .T. ) ;
#4643 = DIRECTION ( 'NONE',  ( 0.000000000000000000, 0.000000000000000000, 1.000000000000000000 ) ) ;
#4644 = DIRECTION ( 'NONE',  ( -1.000000000000000000, 0.000000000000000000, 0.000000000000000000 ) ) ;
#4645 = DIRECTION ( 'NONE',  ( -1.000000000000000000, 0.000000000000000000, -0.000000000000000000 ) ) ;
#4646 = DIRECTION ( 'NONE',  ( -0.000000000000000000, -0.000000000000000000, -1.000000000000000000 ) ) ;
#4647 = DIRECTION ( 'NONE',  ( 1.000000000000000000, 0.000000000000000000, -0.000000000000000000 ) ) ;
#4648 = VERTEX_POINT ( 'NONE', #7711 ) ;
#4649 = DIRECTION ( 'NONE',  ( -1.000000000000000000, 0.000000000000000000, -0.000000000000000000 ) ) ;
#4650 = DIRECTION ( 'NONE',  ( 6.661338147750939243E-16, 1.000000000000000000, 1.196600382587767489E-31 ) ) ;
#4651 = EDGE_CURVE ( 'NONE', #3712, #5164, #5833, .T. ) ;
#4652 = VERTEX_POINT ( 'NONE', #4505 ) ;
#4653 = CARTESIAN_POINT ( 'NONE',  ( 114.9999999999999147, -115.0000000000000000, 8.205133554287239938E-16 ) ) ;
#4654 = LINE ( 'NONE', #7234, #4761 ) ;
#4655 = FACE_OUTER_BOUND ( 'NONE', #1731, .T. ) ;
#4656 = CARTESIAN_POINT ( 'NONE',  ( 124.9999999999997442, -125.0000000000000000, 20.00000000000000000 ) ) ;
#4657 = CIRCLE ( 'NONE', #2878, 5.999999999999984901 ) ;
#4658 = DIRECTION ( 'NONE',  ( -0.000000000000000000, -7.945337353457666666E-18, -1.000000000000000000 ) ) ;
#4659 = CIRCLE ( 'NONE', #3431, 4.999999999999990230 ) ;
#4660 = CARTESIAN_POINT ( 'NONE',  ( 115.0000000000000000, -114.9999999999999716, 10.00000000000000000 ) ) ;
#4661 = ORIENTED_EDGE ( 'NONE', *, *, #8053, .F. ) ;
#4662 = FACE_OUTER_BOUND ( 'NONE', #7403, .T. ) ;
#4663 = DIRECTION ( 'NONE',  ( 1.000000000000000000, 0.000000000000000000, 0.000000000000000000 ) ) ;
#4664 = CIRCLE ( 'NONE', #7239, 5.999999999999991118 ) ;
#4665 = DIRECTION ( 'NONE',  ( 1.000000000000000000, 0.000000000000000000, 0.000000000000000000 ) ) ;
#4666 = ORIENTED_EDGE ( 'NONE', *, *, #6382, .T. ) ;
#4667 = CARTESIAN_POINT ( 'NONE',  ( 3.061616997868377718E-16, -2.499999999999995115, -150.0000000000000000 ) ) ;
#4668 = CARTESIAN_POINT ( 'NONE',  ( -31.74999999999995737, 0.000000000000000000, 5.000000000000035527 ) ) ;
#4669 = CARTESIAN_POINT ( 'NONE',  ( -99.49999999999998579, 1.530808498934191521E-15, -12.50000000000000000 ) ) ;
#4670 = VECTOR ( 'NONE', #3483, 1000.000000000000000 ) ;
#4671 = VERTEX_POINT ( 'NONE', #3285 ) ;
#4672 = EDGE_LOOP ( 'NONE', ( #1044, #2745, #4185 ) ) ;
#4673 = DIRECTION ( 'NONE',  ( 1.000000000000000000, 0.000000000000000000, 0.000000000000000000 ) ) ;
#4674 = ORIENTED_EDGE ( 'NONE', *, *, #5736, .F. ) ;
#4675 = EDGE_CURVE ( 'NONE', #6928, #6306, #1971, .T. ) ;
#4676 = EDGE_CURVE ( 'NONE', #1010, #5315, #1457, .T. ) ;
#4677 = VECTOR ( 'NONE', #5501, 1000.000000000000000 ) ;
#4678 = FACE_BOUND ( 'NONE', #1476, .T. ) ;
#4679 = AXIS2_PLACEMENT_3D ( 'NONE', #2706, #2102, #4644 ) ;
#4680 = CARTESIAN_POINT ( 'NONE',  ( 105.0000000000000000, -105.0000000000000568, 340.0000000000000000 ) ) ;
#4681 = CARTESIAN_POINT ( 'NONE',  ( -108.9999999999999147, 115.0000000000000000, 0.000000000000000000 ) ) ;
#4682 = DIRECTION ( 'NONE',  ( -1.752490724247359037E-17, 1.000000000000000000, 3.853078496550133260E-17 ) ) ;
#4683 = VECTOR ( 'NONE', #3034, 1000.000000000000000 ) ;
#4684 = CARTESIAN_POINT ( 'NONE',  ( 0.000000000000000000, 1.191800603018649864E-15, -100.0000000000000000 ) ) ;
#4685 = EDGE_CURVE ( 'NONE', #4182, #6124, #8293, .T. ) ;
#4686 = DIRECTION ( 'NONE',  ( -1.000000000000000000, 0.000000000000000000, 0.000000000000000000 ) ) ;
#4687 = ADVANCED_FACE ( 'NONE', ( #5071 ), #8252, .T. ) ;
#4688 = LINE ( 'NONE', #2225, #685 ) ;
#4689 = ORIENTED_EDGE ( 'NONE', *, *, #1543, .T. ) ;
#4690 = FACE_OUTER_BOUND ( 'NONE', #4930, .T. ) ;
#4691 = VECTOR ( 'NONE', #2254, 1000.000000000000000 ) ;
#4692 = VERTEX_POINT ( 'NONE', #7788 ) ;
#4693 = CIRCLE ( 'NONE', #8062, 5.999999999999991118 ) ;
#4694 = EDGE_LOOP ( 'NONE', ( #5690, #4239, #2455, #3642, #1602, #6527, #4948, #6942, #2629, #7654 ) ) ;
#4695 = VERTEX_POINT ( 'NONE', #2012 ) ;
#4696 = LINE ( 'NONE', #5996, #7925 ) ;
#4697 = CIRCLE ( 'NONE', #7678, 15.00000000000000000 ) ;
#4698 = EDGE_CURVE ( 'NONE', #2803, #334, #5087, .T. ) ;
#4699 = EDGE_CURVE ( 'NONE', #3768, #6134, #603, .T. ) ;
#4700 = DIRECTION ( 'NONE',  ( -1.000000000000000000, -0.000000000000000000, -0.000000000000000000 ) ) ;
#4701 = PLANE ( 'NONE',  #7643 ) ;
#4702 = AXIS2_PLACEMENT_3D ( 'NONE', #7630, #5808, #5125 ) ;
#4703 = AXIS2_PLACEMENT_3D ( 'NONE', #6548, #7444, #1694 ) ;
#4704 = DIRECTION ( 'NONE',  ( 1.000000000000000000, 0.000000000000000000, 0.000000000000000000 ) ) ;
#4705 = ORIENTED_EDGE ( 'NONE', *, *, #3991, .T. ) ;
#4706 = DIRECTION ( 'NONE',  ( -0.000000000000000000, -0.000000000000000000, 1.000000000000000000 ) ) ;
#4707 = CARTESIAN_POINT ( 'NONE',  ( -95.00000000000000000, 95.00000000000008527, 70.00000000000000000 ) ) ;
#4708 = VECTOR ( 'NONE', #1705, 1000.000000000000000 ) ;
#4709 = ORIENTED_EDGE ( 'NONE', *, *, #5253, .F. ) ;
#4710 = DIRECTION ( 'NONE',  ( -0.000000000000000000, -1.000000000000000000, 1.586032892321652236E-16 ) ) ;
#4711 = DIRECTION ( 'NONE',  ( -0.000000000000000000, -1.000000000000000000, -0.000000000000000000 ) ) ;
#4712 = CARTESIAN_POINT ( 'NONE',  ( -99.99999999999990052, 115.0000000000000000, 0.000000000000000000 ) ) ;
#4713 = CARTESIAN_POINT ( 'NONE',  ( 115.0000000000000000, -115.0000000000000000, 340.0000000000000000 ) ) ;
#4714 = VECTOR ( 'NONE', #4402, 1000.000000000000000 ) ;
#4715 = ORIENTED_EDGE ( 'NONE', *, *, #7209, .T. ) ;
#4716 = CARTESIAN_POINT ( 'NONE',  ( -120.0000000000000000, 120.0000000000000000, -28.00000000000002487 ) ) ;
#4717 = VERTEX_POINT ( 'NONE', #200 ) ;
#4718 = DIRECTION ( 'NONE',  ( -0.000000000000000000, -0.000000000000000000, 1.000000000000000000 ) ) ;
#4719 = CARTESIAN_POINT ( 'NONE',  ( 125.0000000000000000, -125.0000000000000000, 340.0000000000000000 ) ) ;
#4720 = EDGE_CURVE ( 'NONE', #3915, #6329, #7834, .T. ) ;
#4721 = CARTESIAN_POINT ( 'NONE',  ( -1.110223024625156540E-13, -12.50000000000001066, 1.387778780781445676E-14 ) ) ;
#4722 = CARTESIAN_POINT ( 'NONE',  ( -125.0000000000000000, 125.0000000000000568, -9.184850993605156622E-15 ) ) ;
#4723 = CARTESIAN_POINT ( 'NONE',  ( 55.00000000000000000, 55.00000000000000000, 240.0000000000000284 ) ) ;
#4724 = DIRECTION ( 'NONE',  ( -0.000000000000000000, 1.000000000000000000, 1.224646799147353207E-16 ) ) ;
#4725 = DIRECTION ( 'NONE',  ( 0.000000000000000000, 1.000000000000000000, 0.000000000000000000 ) ) ;
#4726 = CARTESIAN_POINT ( 'NONE',  ( 125.0000000000000000, -120.0000000000000000, -28.00000000000002487 ) ) ;
#4727 = DIRECTION ( 'NONE',  ( -1.000000000000000000, -0.000000000000000000, -0.000000000000000000 ) ) ;
#4728 = ORIENTED_EDGE ( 'NONE', *, *, #875, .T. ) ;
#4729 = VERTEX_POINT ( 'NONE', #2823 ) ;
#4730 = DIRECTION ( 'NONE',  ( 1.000000000000000000, 0.000000000000000000, 0.000000000000000000 ) ) ;
#4731 = AXIS2_PLACEMENT_3D ( 'NONE', #2285, #4788, #4752 ) ;
#4732 = ADVANCED_FACE ( 'NONE', ( #3362 ), #7221, .F. ) ;
#4733 = EDGE_CURVE ( 'NONE', #6616, #6102, #2221, .T. ) ;
#4734 = ADVANCED_FACE ( 'NONE', ( #5988 ), #6711, .T. ) ;
#4735 = ORIENTED_EDGE ( 'NONE', *, *, #3236, .T. ) ;
#4736 = CARTESIAN_POINT ( 'NONE',  ( 115.0000000000000000, -115.0000000000000000, 340.0000000000000000 ) ) ;
#4737 = CARTESIAN_POINT ( 'NONE',  ( 0.000000000000000000, 0.000000000000000000, -250.0000000000000000 ) ) ;
#4738 = FILL_AREA_STYLE ('',( #7195 ) ) ;
#4739 = CARTESIAN_POINT ( 'NONE',  ( 125.0000000000000000, -125.0000000000000284, 0.000000000000000000 ) ) ;
#4740 = DIRECTION ( 'NONE',  ( -0.000000000000000000, -0.000000000000000000, 1.000000000000000000 ) ) ;
#4741 = CARTESIAN_POINT ( 'NONE',  ( -94.99999999999997158, -95.00000000000008527, 35.00000000000000000 ) ) ;
#4742 = FILL_AREA_STYLE_COLOUR ( '', #6259 ) ;
#4743 = DIRECTION ( 'NONE',  ( 1.000000000000000000, 0.000000000000000000, 0.000000000000000000 ) ) ;
#4744 = AXIS2_PLACEMENT_3D ( 'NONE', #2569, #7160, #4526 ) ;
#4745 = EDGE_LOOP ( 'NONE', ( #2439, #4637, #1949, #6523 ) ) ;
#4746 = CARTESIAN_POINT ( 'NONE',  ( -114.9999999999999147, -115.0000000000000000, 0.000000000000000000 ) ) ;
#4747 = DIRECTION ( 'NONE',  ( 0.000000000000000000, 1.000000000000000000, -1.266875999117951024E-16 ) ) ;
#4748 = LINE ( 'NONE', #144, #3076 ) ;
#4749 = CARTESIAN_POINT ( 'NONE',  ( 0.000000000000000000, 2.342598717236915373, 4.057499999999997442 ) ) ;
#4750 = PRODUCT_DEFINITION_FORMATION_WITH_SPECIFIED_SOURCE ( 'ANY', '', #6807, .NOT_KNOWN. ) ;
#4751 = DIRECTION ( 'NONE',  ( -0.000000000000000000, -0.000000000000000000, 1.000000000000000000 ) ) ;
#4752 = DIRECTION ( 'NONE',  ( 1.000000000000000000, 0.000000000000000000, 0.000000000000000000 ) ) ;
#4753 = EDGE_CURVE ( 'NONE', #2097, #179, #5953, .T. ) ;
#4754 = ORIENTED_EDGE ( 'NONE', *, *, #6791, .T. ) ;
#4755 = ORIENTED_EDGE ( 'NONE', *, *, #5208, .T. ) ;
#4756 = CARTESIAN_POINT ( 'NONE',  ( 105.0000000000000000, -105.0000000000000568, 340.0000000000000000 ) ) ;
#4757 = ORIENTED_EDGE ( 'NONE', *, *, #8193, .T. ) ;
#4758 = FACE_OUTER_BOUND ( 'NONE', #6514, .T. ) ;
#4759 = ORIENTED_EDGE ( 'NONE', *, *, #1462, .F. ) ;
#4760 = CARTESIAN_POINT ( 'NONE',  ( 6.271675211807171912, 49.60982880777384452, -1.656483108071705068 ) ) ;
#4761 = VECTOR ( 'NONE', #3042, 1000.000000000000000 ) ;
#4762 = FACE_OUTER_BOUND ( 'NONE', #8271, .T. ) ;
#4763 = CARTESIAN_POINT ( 'NONE',  ( 14.30908802125418511, -4.500000000000000000, -128.0000000000000284 ) ) ;
#4764 = DIRECTION ( 'NONE',  ( -6.106226635438364917E-16, -3.853078496550153598E-17, -1.000000000000000000 ) ) ;
#4765 = DIRECTION ( 'NONE',  ( -0.000000000000000000, -0.000000000000000000, 1.000000000000000000 ) ) ;
#4766 = LINE ( 'NONE', #3402, #4986 ) ;
#4767 = VERTEX_POINT ( 'NONE', #2061 ) ;
#4768 =( GEOMETRIC_REPRESENTATION_CONTEXT ( 3 ) GLOBAL_UNCERTAINTY_ASSIGNED_CONTEXT ( ( #6745 ) ) GLOBAL_UNIT_ASSIGNED_CONTEXT ( ( #2929, #1558, #4149 ) ) REPRESENTATION_CONTEXT ( 'NONE', 'WORKASPACE' ) );
#4769 = ORIENTED_EDGE ( 'NONE', *, *, #4254, .F. ) ;
#4770 = LINE ( 'NONE', #212, #5353 ) ;
#4771 = CARTESIAN_POINT ( 'NONE',  ( 5.000000000000000000, 7.027796151710712813, -4.057500000000006324 ) ) ;
#4772 = CARTESIAN_POINT ( 'NONE',  ( 50.00000000000000000, -55.00000000000000000, 240.0000000000000284 ) ) ;
#4773 = EDGE_CURVE ( 'NONE', #6358, #7231, #7269, .T. ) ;
#4774 = ADVANCED_FACE ( 'NONE', ( #893, #4762 ), #2780, .F. ) ;
#4775 = CARTESIAN_POINT ( 'NONE',  ( -11.38780311525837163, -48.68618002971793146, -17.67075055658902016 ) ) ;
#4776 = EDGE_CURVE ( 'NONE', #7369, #5586, #1570, .T. ) ;
#4777 = DIRECTION ( 'NONE',  ( -0.000000000000000000, -0.000000000000000000, 1.000000000000000000 ) ) ;
#4778 = DIRECTION ( 'NONE',  ( -0.000000000000000000, -0.000000000000000000, 1.000000000000000000 ) ) ;
#4779 = ORIENTED_EDGE ( 'NONE', *, *, #8140, .F. ) ;
#4780 = LINE ( 'NONE', #2722, #1800 ) ;
#4781 = CARTESIAN_POINT ( 'NONE',  ( 10.00000000000000000, 54.99999999999997158, -93.74999999999998579 ) ) ;
#4782 = ORIENTED_EDGE ( 'NONE', *, *, #4881, .F. ) ;
#4783 = EDGE_LOOP ( 'NONE', ( #7649, #6161, #7566, #5649 ) ) ;
#4784 = CARTESIAN_POINT ( 'NONE',  ( 5.000000000000000000, -3.513898075855354630, 2.028750000000002718 ) ) ;
#4785 = EDGE_CURVE ( 'NONE', #653, #5879, #3880, .T. ) ;
#4786 = CARTESIAN_POINT ( 'NONE',  ( 120.0000000000000000, 115.0000000000000000, 340.0000000000000000 ) ) ;
#4787 = AXIS2_PLACEMENT_3D ( 'NONE', #3833, #4617, #7085 ) ;
#4788 = DIRECTION ( 'NONE',  ( -0.000000000000000000, -0.000000000000000000, 1.000000000000000000 ) ) ;
#4789 = VERTEX_POINT ( 'NONE', #2173 ) ;
#4790 = CIRCLE ( 'NONE', #1033, 4.999999999999990230 ) ;
#4791 = ORIENTED_EDGE ( 'NONE', *, *, #7075, .F. ) ;
#4792 = CYLINDRICAL_SURFACE ( 'NONE', #4264, 5.499999999999991118 ) ;
#4793 = ORIENTED_EDGE ( 'NONE', *, *, #2164, .T. ) ;
#4794 = LINE ( 'NONE', #2981, #5101 ) ;
#4795 = EDGE_CURVE ( 'NONE', #4444, #2571, #3967, .T. ) ;
#4796 = EDGE_CURVE ( 'NONE', #6622, #2952, #6592, .T. ) ;
#4797 = DIRECTION ( 'NONE',  ( 0.9992060621654691444, -0.03984024763698791605, 1.223674505719567166E-16 ) ) ;
#4798 = CONICAL_SURFACE ( 'NONE', #4124, 4.999999999999990230, 1.029744258676656754 ) ;
#4799 = ORIENTED_EDGE ( 'NONE', *, *, #2172, .T. ) ;
#4800 = DIRECTION ( 'NONE',  ( -1.000000000000000000, -1.460819769243626145E-16, 0.000000000000000000 ) ) ;
#4801 = DIRECTION ( 'NONE',  ( 1.000000000000000000, -1.734723475976806700E-15, 0.000000000000000000 ) ) ;
#4802 = DIRECTION ( 'NONE',  ( -0.000000000000000000, -0.000000000000000000, 1.000000000000000000 ) ) ;
#4803 = DIRECTION ( 'NONE',  ( -1.000000000000000000, -0.000000000000000000, -0.000000000000000000 ) ) ;
#4804 = AXIS2_PLACEMENT_3D ( 'NONE', #6939, #5675, #7452 ) ;
#4805 = CARTESIAN_POINT ( 'NONE',  ( 6.123246359811209136E-15, -49.99999999999999289, -25.00000000000000000 ) ) ;
#4806 = PLANE ( 'NONE',  #5382 ) ;
#4807 = CIRCLE ( 'NONE', #5083, 8.999999999999994671 ) ;
#4808 = ORIENTED_EDGE ( 'NONE', *, *, #2335, .T. ) ;
#4809 = ORIENTED_EDGE ( 'NONE', *, *, #6866, .T. ) ;
#4810 = EDGE_LOOP ( 'NONE', ( #3283, #1901 ) ) ;
#4811 = AXIS2_PLACEMENT_3D ( 'NONE', #7441, #1651, #4200 ) ;
#4812 = EDGE_LOOP ( 'NONE', ( #29, #8137, #6970, #3898 ) ) ;
#4813 = AXIS2_PLACEMENT_3D ( 'NONE', #3501, #5465, #8035 ) ;
#4814 = DIRECTION ( 'NONE',  ( -0.000000000000000000, -0.000000000000000000, 1.000000000000000000 ) ) ;
#4815 = AXIS2_PLACEMENT_3D ( 'NONE', #6335, #553, #2541 ) ;
#4816 = DIRECTION ( 'NONE',  ( 1.000000000000000000, 0.000000000000000000, 0.000000000000000000 ) ) ;
#4817 = EDGE_LOOP ( 'NONE', ( #8087, #935, #5598 ) ) ;
#4818 = CARTESIAN_POINT ( 'NONE',  ( 20.76917701662883076, -5.000000000000000000, 0.000000000000000000 ) ) ;
#4819 =( NAMED_UNIT ( * ) PLANE_ANGLE_UNIT ( ) SI_UNIT ( $, .RADIAN. ) );
#4820 = AXIS2_PLACEMENT_3D ( 'NONE', #4598, #810, #4078 ) ;
#4821 =( NAMED_UNIT ( * ) PLANE_ANGLE_UNIT ( ) SI_UNIT ( $, .RADIAN. ) );
#4822 = DIRECTION ( 'NONE',  ( -0.000000000000000000, -0.000000000000000000, 1.000000000000000000 ) ) ;
#4823 = ORIENTED_EDGE ( 'NONE', *, *, #7229, .T. ) ;
#4824 = AXIS2_PLACEMENT_3D ( 'NONE', #5983, #1395, #149 ) ;
#4825 = EDGE_CURVE ( 'NONE', #1918, #717, #5910, .T. ) ;
#4826 = CARTESIAN_POINT ( 'NONE',  ( 5.000000000000000000, 2.342598717236902939, -4.057500000000001883 ) ) ;
#4827 = ORIENTED_EDGE ( 'NONE', *, *, #4642, .T. ) ;
#4828 = DIRECTION ( 'NONE',  ( -0.000000000000000000, -0.000000000000000000, 1.000000000000000000 ) ) ;
#4829 = CARTESIAN_POINT ( 'NONE',  ( 80.00000000000000000, 0.000000000000000000, 4.171999999999999709 ) ) ;
#4830 = AXIS2_PLACEMENT_3D ( 'NONE', #7377, #4183, #1595 ) ;
#4831 = CIRCLE ( 'NONE', #1214, 5.999999999999984901 ) ;
#4832 = DIRECTION ( 'NONE',  ( 0.000000000000000000, 1.000000000000000000, 0.000000000000000000 ) ) ;
#4833 = ADVANCED_FACE ( 'NONE', ( #5325 ), #3441, .T. ) ;
#4834 = DIRECTION ( 'NONE',  ( 6.106226635438361958E-16, 0.000000000000000000, 1.000000000000000000 ) ) ;
#4835 = ADVANCED_FACE ( 'NONE', ( #246 ), #4040, .T. ) ;
#4836 = EDGE_CURVE ( 'NONE', #67, #448, #78, .T. ) ;
#4837 = EDGE_CURVE ( 'NONE', #5309, #4868, #8338, .T. ) ;
#4838 = CIRCLE ( 'NONE', #1217, 57.99999999999995737 ) ;
#4839 = AXIS2_PLACEMENT_3D ( 'NONE', #6073, #2827, #1492 ) ;
#4840 = ORIENTED_EDGE ( 'NONE', *, *, #7172, .F. ) ;
#4841 = CARTESIAN_POINT ( 'NONE',  ( 1.592040838891560279E-15, -105.0000000000000711, 92.99999999999997158 ) ) ;
#4842 = ORIENTED_EDGE ( 'NONE', *, *, #2768, .F. ) ;
#4843 = CARTESIAN_POINT ( 'NONE',  ( 0.000000000000000000, 125.0000000000000568, 79.99999999999992895 ) ) ;
#4844 = DIRECTION ( 'NONE',  ( 1.224646799147348523E-16, 3.160065852750576588E-30, -1.000000000000000000 ) ) ;
#4845 = VECTOR ( 'NONE', #1371, 1000.000000000000000 ) ;
#4846 = EDGE_LOOP ( 'NONE', ( #3109, #2831, #8156 ) ) ;
#4847 = CARTESIAN_POINT ( 'NONE',  ( 0.000000000000000000, 0.000000000000000000, 250.0000000000000000 ) ) ;
#4848 = EDGE_CURVE ( 'NONE', #8106, #4695, #4330, .T. ) ;
#4849 = CARTESIAN_POINT ( 'NONE',  ( 14.30908802125418511, -4.500000000000000000, -120.5000000000000284 ) ) ;
#4850 = DIRECTION ( 'NONE',  ( 0.000000000000000000, -1.000000000000000000, 1.266875999117951024E-16 ) ) ;
#4851 = VERTEX_POINT ( 'NONE', #6756 ) ;
#4852 = CARTESIAN_POINT ( 'NONE',  ( 115.0000000000000000, 115.0000000000000000, 70.00000000000000000 ) ) ;
#4853 = ORIENTED_EDGE ( 'NONE', *, *, #1136, .T. ) ;
#4854 = DIRECTION ( 'NONE',  ( -0.000000000000000000, -0.000000000000000000, 1.000000000000000000 ) ) ;
#4855 = VERTEX_POINT ( 'NONE', #6930 ) ;
#4856 = VERTEX_POINT ( 'NONE', #5447 ) ;
#4857 = DIRECTION ( 'NONE',  ( 0.000000000000000000, 0.000000000000000000, -1.000000000000000000 ) ) ;
#4858 = CARTESIAN_POINT ( 'NONE',  ( -115.0000000000000284, -115.0000000000000000, 20.00000000000000355 ) ) ;
#4859 = DIRECTION ( 'NONE',  ( 1.000000000000000000, 0.000000000000000000, 0.000000000000000000 ) ) ;
#4860 = ORIENTED_EDGE ( 'NONE', *, *, #1135, .F. ) ;
#4861 = DIRECTION ( 'NONE',  ( -9.992007221626408864E-16, -1.000000000000000000, -0.000000000000000000 ) ) ;
#4862 = CONICAL_SURFACE ( 'NONE', #1786, 4.999999999999990230, 1.029744258676656754 ) ;
#4863 =( NAMED_UNIT ( * ) SI_UNIT ( $, .STERADIAN. ) SOLID_ANGLE_UNIT ( ) );
#4864 = CARTESIAN_POINT ( 'NONE',  ( 99.49999999999998579, 0.000000000000000000, 12.50000000000000000 ) ) ;
#4865 = ORIENTED_EDGE ( 'NONE', *, *, #570, .T. ) ;
#4866 = CARTESIAN_POINT ( 'NONE',  ( 105.0000000000000000, -72.50000000000001421, 240.0000000000000284 ) ) ;
#4867 = CARTESIAN_POINT ( 'NONE',  ( 59.99999999999999289, 55.00000000000000000, 220.0000000000000284 ) ) ;
#4868 = VERTEX_POINT ( 'NONE', #465 ) ;
#4869 = ORIENTED_EDGE ( 'NONE', *, *, #5944, .T. ) ;
#4870 = DIRECTION ( 'NONE',  ( -0.000000000000000000, -0.000000000000000000, 1.000000000000000000 ) ) ;
#4871 = LINE ( 'NONE', #2447, #3565 ) ;
#4872 = EDGE_CURVE ( 'NONE', #5616, #5541, #2377, .T. ) ;
#4873 = ORIENTED_EDGE ( 'NONE', *, *, #1392, .F. ) ;
#4874 = CIRCLE ( 'NONE', #5958, 12.50000000000000000 ) ;
#4875 = FACE_OUTER_BOUND ( 'NONE', #2812, .T. ) ;
#4876 = DIRECTION ( 'NONE',  ( 1.000000000000000000, 0.000000000000000000, 0.000000000000000000 ) ) ;
#4877 = DIRECTION ( 'NONE',  ( -0.000000000000000000, -0.000000000000000000, 1.000000000000000000 ) ) ;
#4878 = PRODUCT_DEFINITION_CONTEXT ( 'detailed design', #6511, 'design' ) ;
#4879 = VERTEX_POINT ( 'NONE', #6242 ) ;
#4880 = CARTESIAN_POINT ( 'NONE',  ( -125.0000000000000000, 125.0000000000000000, 20.00000000000000000 ) ) ;
#4881 = EDGE_CURVE ( 'NONE', #3015, #6124, #5577, .T. ) ;
#4882 = DIRECTION ( 'NONE',  ( 0.000000000000000000, 0.000000000000000000, -1.000000000000000000 ) ) ;
#4883 = ORIENTED_EDGE ( 'NONE', *, *, #3909, .T. ) ;
#4884 = AXIS2_PLACEMENT_3D ( 'NONE', #84, #5254, #7390 ) ;
#4885 = DIRECTION ( 'NONE',  ( 1.000000000000000000, 0.000000000000000000, 0.000000000000000000 ) ) ;
#4886 = ADVANCED_FACE ( 'NONE', ( #4165 ), #8107, .T. ) ;
#4887 = ITEM_DEFINED_TRANSFORMATION ( 'NONE', 'NONE', #7742,  #1299 ) ;
#4888 = EDGE_CURVE ( 'NONE', #1427, #1581, #6710, .T. ) ;
#4889 = ORIENTED_EDGE ( 'NONE', *, *, #5623, .F. ) ;
#4890 = DIRECTION ( 'NONE',  ( -0.000000000000000000, -0.000000000000000000, 1.000000000000000000 ) ) ;
#4891 = CIRCLE ( 'NONE', #1259, 15.00000000000001421 ) ;
#4892 = ORIENTED_EDGE ( 'NONE', *, *, #7590, .F. ) ;
#4893 = LINE ( 'NONE', #6835, #3255 ) ;
#4894 = LINE ( 'NONE', #4928, #6431 ) ;
#4895 = FACE_OUTER_BOUND ( 'NONE', #7516, .T. ) ;
#4896 = CIRCLE ( 'NONE', #6171, 12.99999999999999822 ) ;
#4897 = ORIENTED_EDGE ( 'NONE', *, *, #2685, .T. ) ;
#4898 = ORIENTED_EDGE ( 'NONE', *, *, #5761, .F. ) ;
#4899 = AXIS2_PLACEMENT_3D ( 'NONE', #2103, #818, #4166 ) ;
#4900 = LINE ( 'NONE', #7491, #911 ) ;
#4901 = LINE ( 'NONE', #6726, #2050 ) ;
#4902 = EDGE_CURVE ( 'NONE', #4377, #8051, #4894, .T. ) ;
#4903 = ORIENTED_EDGE ( 'NONE', *, *, #3331, .F. ) ;
#4904 = DIRECTION ( 'NONE',  ( -0.000000000000000000, -0.000000000000000000, 1.000000000000000000 ) ) ;
#4905 = AXIS2_PLACEMENT_3D ( 'NONE', #5381, #3541, #1461 ) ;
#4906 = FACE_OUTER_BOUND ( 'NONE', #859, .T. ) ;
#4907 = CARTESIAN_POINT ( 'NONE',  ( -54.99999999999999289, 55.00000000000000711, 27.50000000000000000 ) ) ;
#4908 = ORIENTED_EDGE ( 'NONE', *, *, #2229, .T. ) ;
#4909 = ORIENTED_EDGE ( 'NONE', *, *, #1439, .F. ) ;
#4910 = CARTESIAN_POINT ( 'NONE',  ( -55.00000000000000000, -55.00000000000000000, 240.0000000000000284 ) ) ;
#4911 = FACE_OUTER_BOUND ( 'NONE', #8148, .T. ) ;
#4912 = CIRCLE ( 'NONE', #6129, 5.000000000000004441 ) ;
#4913 = ORIENTED_EDGE ( 'NONE', *, *, #7184, .T. ) ;
#4914 = FACE_OUTER_BOUND ( 'NONE', #2589, .T. ) ;
#4915 = ORIENTED_EDGE ( 'NONE', *, *, #5965, .F. ) ;
#4916 = DIRECTION ( 'NONE',  ( -1.000000000000000000, -0.000000000000000000, -0.000000000000000000 ) ) ;
#4917 = VERTEX_POINT ( 'NONE', #6793 ) ;
#4918 = DIRECTION ( 'NONE',  ( -0.000000000000000000, -0.000000000000000000, 1.000000000000000000 ) ) ;
#4919 = PLANE ( 'NONE',  #4032 ) ;
#4920 = ORIENTED_EDGE ( 'NONE', *, *, #5820, .F. ) ;
#4921 = PRODUCT_CONTEXT ( 'NONE', #3360, 'mechanical' ) ;
#4922 = EDGE_LOOP ( 'NONE', ( #760, #4715, #4908, #5105 ) ) ;
#4923 = CARTESIAN_POINT ( 'NONE',  ( 4.030269011847453342, 49.83886670901035387, -0.6603997896886467656 ) ) ;
#4924 = DIRECTION ( 'NONE',  ( -0.000000000000000000, 0.000000000000000000, 1.000000000000000000 ) ) ;
#4925 =( GEOMETRIC_REPRESENTATION_CONTEXT ( 3 ) GLOBAL_UNCERTAINTY_ASSIGNED_CONTEXT ( ( #3790 ) ) GLOBAL_UNIT_ASSIGNED_CONTEXT ( ( #6519, #7919, #3379 ) ) REPRESENTATION_CONTEXT ( 'NONE', 'WORKASPACE' ) );
#4926 = ORIENTED_EDGE ( 'NONE', *, *, #8105, .T. ) ;
#4927 = ADVANCED_FACE ( 'NONE', ( #3566 ), #1785, .F. ) ;
#4928 = CARTESIAN_POINT ( 'NONE',  ( -60.99999999999998579, 55.00000000000000711, 27.50000000000000000 ) ) ;
#4929 = ADVANCED_FACE ( 'NONE', ( #3667 ), #4284, .T. ) ;
#4930 = EDGE_LOOP ( 'NONE', ( #1383, #2156, #4281 ) ) ;
#4931 = ORIENTED_EDGE ( 'NONE', *, *, #8169, .F. ) ;
#4932 = CARTESIAN_POINT ( 'NONE',  ( 0.000000000000000000, 0.000000000000000000, 0.000000000000000000 ) ) ;
#4933 = PLANE ( 'NONE',  #5639 ) ;
#4934 = CIRCLE ( 'NONE', #8180, 2.499999999999996003 ) ;
#4935 = ORIENTED_EDGE ( 'NONE', *, *, #5829, .T. ) ;
#4936 = ADVANCED_FACE ( 'NONE', ( #6151, #4976 ), #6838, .T. ) ;
#4937 = ORIENTED_EDGE ( 'NONE', *, *, #1098, .F. ) ;
#4938 = CARTESIAN_POINT ( 'NONE',  ( 0.000000000000000000, -2.342598717236898054, 4.057500000000003659 ) ) ;
#4939 = AXIS2_PLACEMENT_3D ( 'NONE', #6933, #8245, #7613 ) ;
#4940 = EDGE_CURVE ( 'NONE', #6868, #6215, #6025, .T. ) ;
#4941 = CYLINDRICAL_SURFACE ( 'NONE', #2789, 5.000000000000004441 ) ;
#4942 = PLANE ( 'NONE',  #7612 ) ;
#4943 = CARTESIAN_POINT ( 'NONE',  ( -114.9999999999999858, -114.9999999999999858, 20.00000000000000000 ) ) ;
#4944 = CARTESIAN_POINT ( 'NONE',  ( -5.554896158147707652, -49.69628058154707873, -1.272184882194882904 ) ) ;
#4945 =( NAMED_UNIT ( * ) SI_UNIT ( $, .STERADIAN. ) SOLID_ANGLE_UNIT ( ) );
#4946 = AXIS2_PLACEMENT_3D ( 'NONE', #7151, #1377, #6385 ) ;
#4947 = VECTOR ( 'NONE', #2646, 1000.000000000000000 ) ;
#4948 = ORIENTED_EDGE ( 'NONE', *, *, #6929, .F. ) ;
#4949 = ADVANCED_FACE ( 'NONE', ( #5490, #2861 ), #2338, .T. ) ;
#4950 = CARTESIAN_POINT ( 'NONE',  ( 125.0000000000000000, 125.0000000000000568, -9.184850993605156622E-15 ) ) ;
#4951 = VECTOR ( 'NONE', #2261, 1000.000000000000000 ) ;
#4952 = FACE_BOUND ( 'NONE', #593, .T. ) ;
#4953 = AXIS2_PLACEMENT_3D ( 'NONE', #7969, #2203, #5345 ) ;
#4954 = VERTEX_POINT ( 'NONE', #420 ) ;
#4955 = LINE ( 'NONE', #6693, #4019 ) ;
#4956 = EDGE_CURVE ( 'NONE', #5976, #354, #4132, .T. ) ;
#4957 = DIRECTION ( 'NONE',  ( -0.000000000000000000, -0.000000000000000000, 1.000000000000000000 ) ) ;
#4958 = EDGE_LOOP ( 'NONE', ( #3791, #567, #1310, #1577 ) ) ;
#4959 = PRESENTATION_LAYER_ASSIGNMENT (  '', '', ( #5667 ) ) ;
#4960 = VECTOR ( 'NONE', #3992, 1000.000000000000000 ) ;
#4961 = LINE ( 'NONE', #4313, #2917 ) ;
#4962 = ORIENTED_EDGE ( 'NONE', *, *, #3079, .F. ) ;
#4963 = DIRECTION ( 'NONE',  ( 0.000000000000000000, -0.000000000000000000, -1.000000000000000000 ) ) ;
#4964 = VECTOR ( 'NONE', #6958, 999.9999999999998863 ) ;
#4965 = CYLINDRICAL_SURFACE ( 'NONE', #772, 75.00000000000001421 ) ;
#4966 = AXIS2_PLACEMENT_3D ( 'NONE', #2966, #8003, #961 ) ;
#4967 = VERTEX_POINT ( 'NONE', #8059 ) ;
#4968 = DIRECTION ( 'NONE',  ( 0.8571673007021112234, 0.000000000000000000, 0.5150380749100560429 ) ) ;
#4969 = DIRECTION ( 'NONE',  ( -1.000000000000000000, -0.000000000000000000, -0.000000000000000000 ) ) ;
#4970 = ORIENTED_EDGE ( 'NONE', *, *, #1136, .F. ) ;
#4971 = CARTESIAN_POINT ( 'NONE',  ( 8.257771144136533792, 49.31688802671483529, -21.91964719072836587 ) ) ;
#4972 = CONICAL_SURFACE ( 'NONE', #8073, 4.999999999999990230, 1.029744258676656754 ) ;
#4973 = ORIENTED_EDGE ( 'NONE', *, *, #4501, .T. ) ;
#4974 = AXIS2_PLACEMENT_3D ( 'NONE', #4507, #7587, #3287 ) ;
#4975 = ORIENTED_EDGE ( 'NONE', *, *, #5426, .T. ) ;
#4976 = FACE_BOUND ( 'NONE', #5251, .T. ) ;
#4977 = ORIENTED_EDGE ( 'NONE', *, *, #2105, .T. ) ;
#4978 = ORIENTED_EDGE ( 'NONE', *, *, #1413, .F. ) ;
#4979 = CARTESIAN_POINT ( 'NONE',  ( 5.000000000000000000, 4.685197434473814759, -5.637851296924623057E-15 ) ) ;
#4980 = CIRCLE ( 'NONE', #1352, 5.999999999999991118 ) ;
#4981 = CARTESIAN_POINT ( 'NONE',  ( -1.110223024625156540E-13, -12.50000000000001066, 1.387778780781445676E-14 ) ) ;
#4982 = AXIS2_PLACEMENT_3D ( 'NONE', #4852, #2340, #6932 ) ;
#4983 = EDGE_CURVE ( 'NONE', #6772, #2948, #2299, .T. ) ;
#4984 = ORIENTED_EDGE ( 'NONE', *, *, #6588, .F. ) ;
#4985 = ORIENTED_EDGE ( 'NONE', *, *, #7989, .F. ) ;
#4986 = VECTOR ( 'NONE', #1142, 1000.000000000000000 ) ;
#4987 = CYLINDRICAL_SURFACE ( 'NONE', #4208, 12.50000000000000000 ) ;
#4988 = DIRECTION ( 'NONE',  ( 0.000000000000000000, -0.000000000000000000, 1.000000000000000000 ) ) ;
#4989 = CARTESIAN_POINT ( 'NONE',  ( 0.000000000000000000, 0.000000000000000000, 15.00000000000000000 ) ) ;
#4990 = PRODUCT_DEFINITION_SHAPE ( 'NONE', 'NONE',  #8351 ) ;
#4991 = CARTESIAN_POINT ( 'NONE',  ( 5.000000000000000000, 2.342598717236902939, -4.057500000000001883 ) ) ;
#4992 = ORIENTED_EDGE ( 'NONE', *, *, #7798, .F. ) ;
#4993 = CARTESIAN_POINT ( 'NONE',  ( -1.638770961094136114, -49.97482151629360914, -24.89896468147090758 ) ) ;
#4994 = DIRECTION ( 'NONE',  ( 0.000000000000000000, 1.000000000000000000, 0.000000000000000000 ) ) ;
#4995 = EDGE_CURVE ( 'NONE', #1268, #4767, #92, .T. ) ;
#4996 = ADVANCED_FACE ( 'NONE', ( #2990 ), #8151, .F. ) ;
#4997 = EDGE_CURVE ( 'NONE', #7082, #5603, #682, .T. ) ;
#4998 = EDGE_LOOP ( 'NONE', ( #5801, #6492, #994, #6907 ) ) ;
#4999 = LINE ( 'NONE', #1802, #7109 ) ;
#5000 = CYLINDRICAL_SURFACE ( 'NONE', #6597, 8.000000000000000000 ) ;
#5001 = AXIS2_PLACEMENT_3D ( 'NONE', #2986, #4890, #3488 ) ;
#5002 = LINE ( 'NONE', #574, #6046 ) ;
#5003 = CARTESIAN_POINT ( 'NONE',  ( -105.0000000000000000, 105.0000000000000284, 240.0000000000000284 ) ) ;
#5004 = ORIENTED_EDGE ( 'NONE', *, *, #6741, .F. ) ;
#5005 = LINE ( 'NONE', #3738, #8048 ) ;
#5006 = DIRECTION ( 'NONE',  ( -0.000000000000000000, -0.000000000000000000, 1.000000000000000000 ) ) ;
#5007 = VERTEX_POINT ( 'NONE', #7011 ) ;
#5008 = LINE ( 'NONE', #4361, #2160 ) ;
#5009 = ORIENTED_EDGE ( 'NONE', *, *, #7439, .F. ) ;
#5010 = DIRECTION ( 'NONE',  ( -0.000000000000000000, 1.000000000000000000, -1.266875999117951024E-16 ) ) ;
#5011 = CARTESIAN_POINT ( 'NONE',  ( 0.000000000000000000, 2.499999999999990230, -250.0000000000000000 ) ) ;
#5012 = APPLICATION_PROTOCOL_DEFINITION ( 'draft international standard', 'automotive_design', 1998, #2370 ) ;
#5013 = EDGE_CURVE ( 'NONE', #7975, #3837, #5825, .T. ) ;
#5014 = LINE ( 'NONE', #4326, #8102 ) ;
#5015 = AXIS2_PLACEMENT_3D ( 'NONE', #6050, #7371, #265 ) ;
#5016 = ORIENTED_EDGE ( 'NONE', *, *, #1817, .F. ) ;
#5017 = CARTESIAN_POINT ( 'NONE',  ( 1.530808498934191521E-15, -125.0000000000000000, 0.000000000000000000 ) ) ;
#5018 = VERTEX_POINT ( 'NONE', #1270 ) ;
#5019 = ORIENTED_EDGE ( 'NONE', *, *, #7898, .F. ) ;
#5020 = FACE_OUTER_BOUND ( 'NONE', #1951, .T. ) ;
#5021 = CARTESIAN_POINT ( 'NONE',  ( -114.9999999999999147, -100.0000000000000000, 0.000000000000000000 ) ) ;
#5022 = AXIS2_PLACEMENT_3D ( 'NONE', #4721, #6670, #1650 ) ;
#5023 =( GEOMETRIC_REPRESENTATION_CONTEXT ( 3 ) GLOBAL_UNCERTAINTY_ASSIGNED_CONTEXT ( ( #6995 ) ) GLOBAL_UNIT_ASSIGNED_CONTEXT ( ( #5461, #958, #3499 ) ) REPRESENTATION_CONTEXT ( 'NONE', 'WORKASPACE' ) );
#5024 = VERTEX_POINT ( 'NONE', #5789 ) ;
#5025 = ORIENTED_EDGE ( 'NONE', *, *, #7844, .F. ) ;
#5026 = CARTESIAN_POINT ( 'NONE',  ( 0.000000000000000000, 125.0000000000000000, -12.50000000000000000 ) ) ;
#5027 = DIRECTION ( 'NONE',  ( 1.000000000000000000, 0.000000000000000000, 0.000000000000000000 ) ) ;
#5028 = EDGE_CURVE ( 'NONE', #6392, #4671, #868, .T. ) ;
#5029 = PLANE ( 'NONE',  #7006 ) ;
#5030 = EDGE_LOOP ( 'NONE', ( #6049, #3052, #2945, #2771, #3206 ) ) ;
#5031 = FILL_AREA_STYLE_COLOUR ( '', #3723 ) ;
#5032 = DIRECTION ( 'NONE',  ( -0.3875026790906691554, 2.505883310333456634E-16, -0.9218685772373164111 ) ) ;
#5033 = AXIS2_PLACEMENT_3D ( 'NONE', #7353, #1447, #979 ) ;
#5034 = PRODUCT_RELATED_PRODUCT_CATEGORY ( 'part', '', ( #2884 ) ) ;
#5035 = CARTESIAN_POINT ( 'NONE',  ( 75.00000000000001421, 9.184850993605150311E-15, 15.00000000000000000 ) ) ;
#5036 = EDGE_CURVE ( 'NONE', #3000, #900, #1236, .T. ) ;
#5037 = AXIS2_PLACEMENT_3D ( 'NONE', #2898, #2782, #7942 ) ;
#5038 = EDGE_CURVE ( 'NONE', #5777, #416, #3759, .T. ) ;
#5039 = PLANE ( 'NONE',  #2560 ) ;
#5040 = ADVANCED_FACE ( 'NONE', ( #4459 ), #1531, .T. ) ;
#5041 = FACE_OUTER_BOUND ( 'NONE', #5112, .T. ) ;
#5042 = FACE_OUTER_BOUND ( 'NONE', #1671, .T. ) ;
#5043 = CARTESIAN_POINT ( 'NONE',  ( 3.256071768936471766, -49.89543388580304395, -0.4244881437574537508 ) ) ;
#5044 = DIRECTION ( 'NONE',  ( -0.000000000000000000, -7.945337353457666666E-18, -1.000000000000000000 ) ) ;
#5045 = DIRECTION ( 'NONE',  ( 0.000000000000000000, 0.000000000000000000, 1.000000000000000000 ) ) ;
#5046 = VECTOR ( 'NONE', #2566, 1000.000000000000000 ) ;
#5047 = ORIENTED_EDGE ( 'NONE', *, *, #4675, .F. ) ;
#5048 = EDGE_CURVE ( 'NONE', #3350, #3250, #5095, .T. ) ;
#5049 = ORIENTED_EDGE ( 'NONE', *, *, #737, .T. ) ;
#5050 = CARTESIAN_POINT ( 'NONE',  ( 5.000000000000000000, 4.685197434473814759, -5.637851296924623057E-15 ) ) ;
#5051 = ORIENTED_EDGE ( 'NONE', *, *, #512, .F. ) ;
#5052 = CARTESIAN_POINT ( 'NONE',  ( 75.00000000000001421, 9.184850993605150311E-15, 57.99999999999999289 ) ) ;
#5053 = LINE ( 'NONE', #7644, #1766 ) ;
#5054 = EDGE_LOOP ( 'NONE', ( #1344, #6656, #5687, #7794, #1331 ) ) ;
#5055 = CARTESIAN_POINT ( 'NONE',  ( 9.920587673301477949, 49.00664693364542046, -20.11565191071547787 ) ) ;
#5056 = PRODUCT ( 'Drive Unit', 'Drive Unit', '', ( #5531 ) ) ;
#5057 = VERTEX_POINT ( 'NONE', #6404 ) ;
#5058 = EDGE_CURVE ( 'NONE', #57, #758, #6451, .T. ) ;
#5059 = DIRECTION ( 'NONE',  ( -1.752490724247359037E-17, 1.000000000000000000, 3.853078496550133260E-17 ) ) ;
#5060 = EDGE_CURVE ( 'NONE', #4375, #7541, #7655, .T. ) ;
#5061 = ORIENTED_EDGE ( 'NONE', *, *, #7530, .T. ) ;
#5062 = AXIS2_PLACEMENT_3D ( 'NONE', #4293, #7450, #6889 ) ;
#5063 = EDGE_LOOP ( 'NONE', ( #267, #7039, #2411, #517 ) ) ;
#5064 = EDGE_CURVE ( 'NONE', #334, #2803, #1881, .T. ) ;
#5065 = AXIS2_PLACEMENT_3D ( 'NONE', #535, #5849, #659 ) ;
#5066 = CARTESIAN_POINT ( 'NONE',  ( -9.130470200569520856, 49.16013940401185778, -3.953130373342527815 ) ) ;
#5067 = DIRECTION ( 'NONE',  ( -1.000000000000000000, -0.000000000000000000, -0.000000000000000000 ) ) ;
#5068 = FACE_OUTER_BOUND ( 'NONE', #5236, .T. ) ;
#5069 = EDGE_LOOP ( 'NONE', ( #7950, #5092, #1994 ) ) ;
#5070 = DIRECTION ( 'NONE',  ( -1.000000000000000000, 0.000000000000000000, 0.000000000000000000 ) ) ;
#5071 = FACE_OUTER_BOUND ( 'NONE', #1295, .T. ) ;
#5072 = DIRECTION ( 'NONE',  ( -0.000000000000000000, -0.000000000000000000, -1.000000000000000000 ) ) ;
#5073 = DIRECTION ( 'NONE',  ( 0.000000000000000000, 0.000000000000000000, -1.000000000000000000 ) ) ;
#5074 = COLOUR_RGB ( '',0.7921568627450980005, 0.8196078431372548767, 0.9333333333333333481 ) ;
#5075 = FACE_BOUND ( 'NONE', #4620, .T. ) ;
#5076 = ORIENTED_EDGE ( 'NONE', *, *, #840, .F. ) ;
#5077 = AXIS2_PLACEMENT_3D ( 'NONE', #7705, #4465, #3084 ) ;
#5078 = CARTESIAN_POINT ( 'NONE',  ( -121.0000000000000284, -115.0000000000000000, 20.00000000000000355 ) ) ;
#5079 = AXIS2_PLACEMENT_3D ( 'NONE', #5458, #4013, #1539 ) ;
#5080 = DIRECTION ( 'NONE',  ( 0.000000000000000000, 1.000000000000000000, 0.000000000000000000 ) ) ;
#5081 = CARTESIAN_POINT ( 'NONE',  ( 11.23255197390109217, -48.72302474870180333, -6.955105218463169869 ) ) ;
#5082 = DIRECTION ( 'NONE',  ( -0.000000000000000000, -0.000000000000000000, 1.000000000000000000 ) ) ;
#5083 = AXIS2_PLACEMENT_3D ( 'NONE', #4660, #5173, #5850 ) ;
#5084 = CARTESIAN_POINT ( 'NONE',  ( -105.9999999999999858, -114.9999999999999858, 20.00000000000000000 ) ) ;
#5085 = EDGE_CURVE ( 'NONE', #509, #3826, #2623, .T. ) ;
#5086 = ORIENTED_EDGE ( 'NONE', *, *, #131, .F. ) ;
#5087 = CIRCLE ( 'NONE', #8204, 2.499999999999984013 ) ;
#5088 = ORIENTED_EDGE ( 'NONE', *, *, #3950, .T. ) ;
#5089 = VECTOR ( 'NONE', #7251, 1000.000000000000000 ) ;
#5090 = VERTEX_POINT ( 'NONE', #2584 ) ;
#5091 = CARTESIAN_POINT ( 'NONE',  ( 99.99999999999991473, -115.0000000000000000, 250.0000000000000000 ) ) ;
#5092 = ORIENTED_EDGE ( 'NONE', *, *, #4795, .T. ) ;
#5093 = CYLINDRICAL_SURFACE ( 'NONE', #7401, 75.00000000000001421 ) ;
#5094 = CARTESIAN_POINT ( 'NONE',  ( 60.99999999999998579, -55.00000000000000711, 27.50000000000000000 ) ) ;
#5095 = CIRCLE ( 'NONE', #5369, 95.00000000000001421 ) ;
#5096 = ITEM_DEFINED_TRANSFORMATION ( 'NONE', 'NONE', #3945,  #1299 ) ;
#5097 = AXIS2_PLACEMENT_3D ( 'NONE', #3623, #4854, #2995 ) ;
#5098 = CARTESIAN_POINT ( 'NONE',  ( 10.61457161467473398, 48.86086578770957800, -19.11406644883056316 ) ) ;
#5099 = ADVANCED_FACE ( 'NONE', ( #5188 ), #7782, .T. ) ;
#5100 = EDGE_CURVE ( 'NONE', #354, #6267, #4541, .T. ) ;
#5101 = VECTOR ( 'NONE', #7388, 1000.000000000000000 ) ;
#5102 = CIRCLE ( 'NONE', #1066, 12.50000000000000000 ) ;
#5103 = ORIENTED_EDGE ( 'NONE', *, *, #3549, .F. ) ;
#5104 = CARTESIAN_POINT ( 'NONE',  ( 108.9999999999999147, -115.0000000000000000, 0.000000000000000000 ) ) ;
#5105 = ORIENTED_EDGE ( 'NONE', *, *, #863, .T. ) ;
#5106 = APPLICATION_CONTEXT ( 'automotive_design' ) ;
#5107 = FACE_OUTER_BOUND ( 'NONE', #4812, .T. ) ;
#5108 = AXIS2_PLACEMENT_3D ( 'NONE', #7676, #10, #2604 ) ;
#5109 = VECTOR ( 'NONE', #7144, 1000.000000000000000 ) ;
#5110 = CARTESIAN_POINT ( 'NONE',  ( -1.632468168883555837, 49.97996006834706151, -24.92059050027006606 ) ) ;
#5111 = DIRECTION ( 'NONE',  ( 1.000000000000000000, 0.000000000000000000, 0.000000000000000000 ) ) ;
#5112 = EDGE_LOOP ( 'NONE', ( #4992, #3557, #4909, #4842 ) ) ;
#5113 = DIRECTION ( 'NONE',  ( -0.000000000000000000, -0.000000000000000000, 1.000000000000000000 ) ) ;
#5114 = CARTESIAN_POINT ( 'NONE',  ( 0.000000000000000000, -4.500000000000000000, -28.00000000000002487 ) ) ;
#5115 = DIRECTION ( 'NONE',  ( -0.000000000000000000, 0.000000000000000000, 1.000000000000000000 ) ) ;
#5116 = AXIS2_PLACEMENT_3D ( 'NONE', #467, #422, #8063 ) ;
#5117 = FACE_OUTER_BOUND ( 'NONE', #7436, .T. ) ;
#5118 = EDGE_LOOP ( 'NONE', ( #2928, #6363, #887, #4562 ) ) ;
#5119 = CARTESIAN_POINT ( 'NONE',  ( 0.000000000000000000, 37.50000000000000000, -100.0000000000000000 ) ) ;
#5120 = DIRECTION ( 'NONE',  ( -0.9873608237139798183, 6.577144320600713862E-16, 0.1584884973581717482 ) ) ;
#5121 = AXIS2_PLACEMENT_3D ( 'NONE', #7560, #2459, #251 ) ;
#5122 = ORIENTED_EDGE ( 'NONE', *, *, #6299, .F. ) ;
#5123 = FACE_OUTER_BOUND ( 'NONE', #8185, .T. ) ;
#5124 = DIRECTION ( 'NONE',  ( 1.000000000000000000, 0.000000000000000000, 0.000000000000000000 ) ) ;
#5125 = DIRECTION ( 'NONE',  ( 0.000000000000000000, 0.000000000000000000, -1.000000000000000000 ) ) ;
#5126 = CARTESIAN_POINT ( 'NONE',  ( 12.47905948369885998, -48.41771210405730130, -13.33173448961934504 ) ) ;
#5127 = DIRECTION ( 'NONE',  ( 0.000000000000000000, 2.960594732333750610E-16, -1.000000000000000000 ) ) ;
#5128 = PRODUCT ( 'Bearing Housing', 'Bearing Housing', '', ( #2499 ) ) ;
#5129 = LINE ( 'NONE', #7729, #4253 ) ;
#5130 = ORIENTED_EDGE ( 'NONE', *, *, #1188, .F. ) ;
#5131 =( NAMED_UNIT ( * ) PLANE_ANGLE_UNIT ( ) SI_UNIT ( $, .RADIAN. ) );
#5132 = CARTESIAN_POINT ( 'NONE',  ( 114.9999999999999147, -100.0000000000000000, 0.000000000000000000 ) ) ;
#5133 = ORIENTED_EDGE ( 'NONE', *, *, #1542, .T. ) ;
#5134 = ORIENTED_EDGE ( 'NONE', *, *, #7716, .T. ) ;
#5135 = DIRECTION ( 'NONE',  ( -0.000000000000000000, -0.000000000000000000, -1.000000000000000000 ) ) ;
#5136 = ORIENTED_EDGE ( 'NONE', *, *, #8326, .F. ) ;
#5137 = ADVANCED_FACE ( 'NONE', ( #7744 ), #1961, .F. ) ;
#5138 = DIRECTION ( 'NONE',  ( -1.000000000000000000, -0.000000000000000000, -0.000000000000000000 ) ) ;
#5139 = CARTESIAN_POINT ( 'NONE',  ( 115.0000000000000284, -115.0000000000000000, 70.00000000000000000 ) ) ;
#5140 = VECTOR ( 'NONE', #6576, 1000.000000000000000 ) ;
#5141 = ORIENTED_EDGE ( 'NONE', *, *, #2429, .F. ) ;
#5142 = CARTESIAN_POINT ( 'NONE',  ( 1.638770961094149436, 49.97482151629360203, -24.89896468147090403 ) ) ;
#5143 = ORIENTED_EDGE ( 'NONE', *, *, #4092, .T. ) ;
#5144 = ORIENTED_EDGE ( 'NONE', *, *, #8324, .F. ) ;
#5145 = CARTESIAN_POINT ( 'NONE',  ( 125.0000000000000000, -125.0000000000000284, 0.000000000000000000 ) ) ;
#5146 = DIRECTION ( 'NONE',  ( 1.000000000000000000, 0.000000000000000000, 0.000000000000000000 ) ) ;
#5147 = VERTEX_POINT ( 'NONE', #5017 ) ;
#5148 = EDGE_LOOP ( 'NONE', ( #6039, #4920, #7842, #1697 ) ) ;
#5149 = EDGE_CURVE ( 'NONE', #8000, #6145, #236, .T. ) ;
#5150 = CARTESIAN_POINT ( 'NONE',  ( -104.9999999999999432, -105.0000000000000853, 340.0000000000000000 ) ) ;
#5151 = ADVANCED_FACE ( 'NONE', ( #3710 ), #8284, .F. ) ;
#5152 = EDGE_CURVE ( 'NONE', #6778, #6841, #3080, .T. ) ;
#5153 = EDGE_LOOP ( 'NONE', ( #2533, #7421, #99, #6130 ) ) ;
#5154 = CARTESIAN_POINT ( 'NONE',  ( -12.07731880710695904, 48.51961889015782958, -15.74894529186713221 ) ) ;
#5155 = CIRCLE ( 'NONE', #1519, 5.499999999999991118 ) ;
#5156 = DIRECTION ( 'NONE',  ( 1.000000000000000000, 0.000000000000000000, 0.000000000000000000 ) ) ;
#5157 = ORIENTED_EDGE ( 'NONE', *, *, #4211, .T. ) ;
#5158 = DIRECTION ( 'NONE',  ( -0.000000000000000000, -1.000000000000000000, -1.224646799147353207E-16 ) ) ;
#5159 = EDGE_CURVE ( 'NONE', #471, #3015, #2813, .T. ) ;
#5160 = DIRECTION ( 'NONE',  ( 0.000000000000000000, 0.000000000000000000, -1.000000000000000000 ) ) ;
#5161 = VERTEX_POINT ( 'NONE', #5865 ) ;
#5162 = CARTESIAN_POINT ( 'NONE',  ( -5.541544814107227879, -49.69330507166043276, -23.71206720076232699 ) ) ;
#5163 = DIRECTION ( 'NONE',  ( -0.3875026790906691554, 1.459681852512834469E-16, -0.9218685772373163001 ) ) ;
#5164 = VERTEX_POINT ( 'NONE', #5234 ) ;
#5165 = ORIENTED_EDGE ( 'NONE', *, *, #5679, .F. ) ;
#5166 = DIRECTION ( 'NONE',  ( 0.000000000000000000, -1.000000000000000000, 0.000000000000000000 ) ) ;
#5167 = DIRECTION ( 'NONE',  ( 1.000000000000000000, 0.000000000000000000, 0.000000000000000000 ) ) ;
#5168 = EDGE_CURVE ( 'NONE', #5293, #5777, #5242, .T. ) ;
#5169 = FACE_OUTER_BOUND ( 'NONE', #7025, .T. ) ;
#5170 = CARTESIAN_POINT ( 'NONE',  ( 102.5000000000000000, 0.000000000000000000, 0.000000000000000000 ) ) ;
#5171 = VECTOR ( 'NONE', #1571, 1000.000000000000000 ) ;
#5172 = DIRECTION ( 'NONE',  ( 1.000000000000000000, 0.000000000000000000, 0.000000000000000000 ) ) ;
#5173 = DIRECTION ( 'NONE',  ( -0.000000000000000000, -0.000000000000000000, 1.000000000000000000 ) ) ;
#5174 = ORIENTED_EDGE ( 'NONE', *, *, #3345, .F. ) ;
#5175 = AXIS2_PLACEMENT_3D ( 'NONE', #7557, #4318, #6920 ) ;
#5176 = ORIENTED_EDGE ( 'NONE', *, *, #3022, .T. ) ;
#5177 = ORIENTED_EDGE ( 'NONE', *, *, #4631, .T. ) ;
#5178 = DIRECTION ( 'NONE',  ( -0.000000000000000000, -0.000000000000000000, 1.000000000000000000 ) ) ;
#5179 = VERTEX_POINT ( 'NONE', #109 ) ;
#5180 = DIRECTION ( 'NONE',  ( 1.000000000000000000, 0.000000000000000000, 0.000000000000000000 ) ) ;
#5181 = DIRECTION ( 'NONE',  ( -0.000000000000000000, -0.000000000000000000, 1.000000000000000000 ) ) ;
#5182 = CYLINDRICAL_SURFACE ( 'NONE', #2645, 5.499999999999991118 ) ;
#5183 = CIRCLE ( 'NONE', #1417, 5.499999999999991118 ) ;
#5184 = CONTEXT_DEPENDENT_SHAPE_REPRESENTATION ( #30, #756 ) ;
#5185 = CARTESIAN_POINT ( 'NONE',  ( -99.49999999999998579, 0.000000000000000000, 0.000000000000000000 ) ) ;
#5186 = VERTEX_POINT ( 'NONE', #7302 ) ;
#5187 = CARTESIAN_POINT ( 'NONE',  ( 0.000000000000000000, -125.0000000000000568, 66.99999999999997158 ) ) ;
#5188 = FACE_OUTER_BOUND ( 'NONE', #6843, .T. ) ;
#5189 = EDGE_LOOP ( 'NONE', ( #3019, #5568 ) ) ;
#5190 = DIRECTION ( 'NONE',  ( 2.643388153869419325E-16, -1.000000000000000000, -0.000000000000000000 ) ) ;
#5191 = ORIENTED_EDGE ( 'NONE', *, *, #4577, .F. ) ;
#5192 = ADVANCED_FACE ( 'NONE', ( #3923 ), #6623, .F. ) ;
#5193 = COLOUR_RGB ( '',0.7921568627450980005, 0.8196078431372548767, 0.9333333333333333481 ) ;
#5194 = CYLINDRICAL_SURFACE ( 'NONE', #6038, 5.000000000000004441 ) ;
#5195 = LINE ( 'NONE', #600, #7865 ) ;
#5196 = ADVANCED_FACE ( 'NONE', ( #5945 ), #2799, .T. ) ;
#5197 = CARTESIAN_POINT ( 'NONE',  ( 4.592425496802574367E-15, -37.50000000000000000, -100.0000000000000000 ) ) ;
#5198 = DIRECTION ( 'NONE',  ( -0.000000000000000000, -0.000000000000000000, 1.000000000000000000 ) ) ;
#5199 = DIRECTION ( 'NONE',  ( 0.000000000000000000, 0.000000000000000000, 1.000000000000000000 ) ) ;
#5200 = DIRECTION ( 'NONE',  ( 0.000000000000000000, 0.000000000000000000, -1.000000000000000000 ) ) ;
#5201 = DIRECTION ( 'NONE',  ( 0.000000000000000000, 0.000000000000000000, 1.000000000000000000 ) ) ;
#5202 = ORIENTED_EDGE ( 'NONE', *, *, #8009, .F. ) ;
#5203 = DIRECTION ( 'NONE',  ( 0.000000000000000000, 0.000000000000000000, 1.000000000000000000 ) ) ;
#5204 = DIRECTION ( 'NONE',  ( -0.9117682355627076962, -0.4107051066384089233, -0.000000000000000000 ) ) ;
#5205 = EDGE_LOOP ( 'NONE', ( #3894, #6954 ) ) ;
#5206 = EDGE_CURVE ( 'NONE', #5879, #653, #4403, .T. ) ;
#5207 = EDGE_CURVE ( 'NONE', #3250, #877, #3275, .T. ) ;
#5208 = EDGE_CURVE ( 'NONE', #8191, #4076, #928, .T. ) ;
#5209 = CYLINDRICAL_SURFACE ( 'NONE', #4946, 20.00000000000000355 ) ;
#5210 = CARTESIAN_POINT ( 'NONE',  ( -10.00000000000000000, -3.448762466456902719E-14, 93.74999999999998579 ) ) ;
#5211 = CARTESIAN_POINT ( 'NONE',  ( 54.99999999999999289, -55.00000000000000711, 27.50000000000000000 ) ) ;
#5212 = CARTESIAN_POINT ( 'NONE',  ( 9.920332936303610794, -49.00669811220510041, -4.884022838024439928 ) ) ;
#5213 = DIRECTION ( 'NONE',  ( -0.000000000000000000, -0.000000000000000000, -1.000000000000000000 ) ) ;
#5214 = CARTESIAN_POINT ( 'NONE',  ( -115.0000000000000284, -115.0000000000000000, 70.00000000000000000 ) ) ;
#5215 = ADVANCED_FACE ( 'NONE', ( #5316 ), #6578, .F. ) ;
#5216 = ORIENTED_EDGE ( 'NONE', *, *, #7636, .F. ) ;
#5217 = EDGE_CURVE ( 'NONE', #1087, #2241, #7533, .T. ) ;
#5218 = DIRECTION ( 'NONE',  ( 0.000000000000000000, 0.000000000000000000, -1.000000000000000000 ) ) ;
#5219 = APPLICATION_CONTEXT ( 'automotive_design' ) ;
#5220 = VECTOR ( 'NONE', #450, 1000.000000000000000 ) ;
#5221 = ORIENTED_EDGE ( 'NONE', *, *, #1357, .T. ) ;
#5222 = EDGE_LOOP ( 'NONE', ( #8166, #6764, #5619, #6255, #2557 ) ) ;
#5223 = DIRECTION ( 'NONE',  ( 0.000000000000000000, 0.000000000000000000, -1.000000000000000000 ) ) ;
#5224 = EDGE_CURVE ( 'NONE', #1294, #1087, #1477, .T. ) ;
#5225 = AXIS2_PLACEMENT_3D ( 'NONE', #1293, #6429, #5886 ) ;
#5226 = ORIENTED_EDGE ( 'NONE', *, *, #6227, .F. ) ;
#5227 = CYLINDRICAL_SURFACE ( 'NONE', #2027, 12.50000000000000000 ) ;
#5228 = LINE ( 'NONE', #1152, #6433 ) ;
#5229 = ITEM_DEFINED_TRANSFORMATION ( 'NONE', 'NONE', #26,  #1299 ) ;
#5230 = CIRCLE ( 'NONE', #5633, 12.99999999999999822 ) ;
#5231 = DIRECTION ( 'NONE',  ( -0.000000000000000000, -0.000000000000000000, 1.000000000000000000 ) ) ;
#5232 = VECTOR ( 'NONE', #1557, 1000.000000000000000 ) ;
#5233 = VERTEX_POINT ( 'NONE', #4035 ) ;
#5234 = CARTESIAN_POINT ( 'NONE',  ( -125.0000000000000000, 120.0000000000000000, -28.00000000000002487 ) ) ;
#5235 = VECTOR ( 'NONE', #3526, 1000.000000000000000 ) ;
#5236 = EDGE_LOOP ( 'NONE', ( #1287, #3780, #5743 ) ) ;
#5237 = LINE ( 'NONE', #5280, #679 ) ;
#5238 = VECTOR ( 'NONE', #5834, 1000.000000000000000 ) ;
#5239 = DIRECTION ( 'NONE',  ( 0.000000000000000000, 1.000000000000000000, 0.000000000000000000 ) ) ;
#5240 = CARTESIAN_POINT ( 'NONE',  ( -102.5000000000000000, 0.000000000000000000, 0.000000000000000000 ) ) ;
#5241 = AXIS2_PLACEMENT_3D ( 'NONE', #2805, #7968, #6618 ) ;
#5242 = CIRCLE ( 'NONE', #4824, 12.99999999999999822 ) ;
#5243 = CARTESIAN_POINT ( 'NONE',  ( -54.99999999999999289, -55.00000000000000711, -27.50000000000000000 ) ) ;
#5244 = FACE_BOUND ( 'NONE', #3060, .T. ) ;
#5245 = DIRECTION ( 'NONE',  ( -0.8571673007021116675, 1.049727191138617833E-16, 0.5150380749100552658 ) ) ;
#5246 = LINE ( 'NONE', #7182, #6185 ) ;
#5247 = AXIS2_PLACEMENT_3D ( 'NONE', #2562, #7725, #2446 ) ;
#5248 = VECTOR ( 'NONE', #5135, 1000.000000000000000 ) ;
#5249 = DIRECTION ( 'NONE',  ( -1.000000000000000000, -0.000000000000000000, -0.000000000000000000 ) ) ;
#5250 = ADVANCED_FACE ( 'NONE', ( #1434 ), #7935, .T. ) ;
#5251 = EDGE_LOOP ( 'NONE', ( #7010, #3423, #6746, #6280, #5573 ) ) ;
#5252 = DIRECTION ( 'NONE',  ( 1.000000000000000000, 0.000000000000000000, 0.000000000000000000 ) ) ;
#5253 = EDGE_CURVE ( 'NONE', #6149, #3213, #4593, .T. ) ;
#5254 = DIRECTION ( 'NONE',  ( 0.8845137860364626903, -0.4665140537126858944, 0.000000000000000000 ) ) ;
#5255 = FACE_OUTER_BOUND ( 'NONE', #5731, .T. ) ;
#5256 = ORIENTED_EDGE ( 'NONE', *, *, #6708, .T. ) ;
#5257 = AXIS2_PLACEMENT_3D ( 'NONE', #3167, #5754, #2554 ) ;
#5258 = DIRECTION ( 'NONE',  ( 1.000000000000000000, 0.000000000000000000, 0.000000000000000000 ) ) ;
#5259 = CARTESIAN_POINT ( 'NONE',  ( 55.00000000000000000, -55.00000000000000000, 240.0000000000000284 ) ) ;
#5260 = EDGE_CURVE ( 'NONE', #5164, #381, #105, .T. ) ;
#5261 = EDGE_CURVE ( 'NONE', #1962, #6239, #2930, .T. ) ;
#5262 = DIRECTION ( 'NONE',  ( -1.000000000000000000, 0.000000000000000000, 0.000000000000000000 ) ) ;
#5263 = EDGE_CURVE ( 'NONE', #1889, #7860, #3433, .T. ) ;
#5264 = AXIS2_PLACEMENT_3D ( 'NONE', #1532, #4727, #5571 ) ;
#5265 = CARTESIAN_POINT ( 'NONE',  ( 99.99999999999990052, 115.0000000000000000, 250.0000000000000000 ) ) ;
#5266 = DIRECTION ( 'NONE',  ( 1.000000000000000000, 0.000000000000000000, 0.000000000000000000 ) ) ;
#5267 = ORIENTED_EDGE ( 'NONE', *, *, #4956, .T. ) ;
#5268 = DIRECTION ( 'NONE',  ( 1.000000000000000000, 0.000000000000000000, 0.000000000000000000 ) ) ;
#5269 = ORIENTED_EDGE ( 'NONE', *, *, #1273, .T. ) ;
#5270 = DIRECTION ( 'NONE',  ( -0.000000000000000000, -0.000000000000000000, -1.000000000000000000 ) ) ;
#5271 = VERTEX_POINT ( 'NONE', #5397 ) ;
#5272 = DIRECTION ( 'NONE',  ( -0.000000000000000000, -0.000000000000000000, 1.000000000000000000 ) ) ;
#5273 = FACE_OUTER_BOUND ( 'NONE', #1238, .T. ) ;
#5274 = EDGE_CURVE ( 'NONE', #6076, #2040, #2660, .T. ) ;
#5275 = CONTEXT_DEPENDENT_SHAPE_REPRESENTATION ( #3313, #476 ) ;
#5276 = CARTESIAN_POINT ( 'NONE',  ( 17.61817604250836311, 4.500000000000000000, -126.0000000000000284 ) ) ;
#5277 = DIRECTION ( 'NONE',  ( 0.8571673007021116675, 0.000000000000000000, 0.5150380749100552658 ) ) ;
#5278 = DIRECTION ( 'NONE',  ( 1.000000000000000000, 0.000000000000000000, 0.000000000000000000 ) ) ;
#5279 = ORIENTED_EDGE ( 'NONE', *, *, #7906, .T. ) ;
#5280 = CARTESIAN_POINT ( 'NONE',  ( -50.00000000000000711, -55.00000000000000000, 220.0000000000000284 ) ) ;
#5281 = EDGE_CURVE ( 'NONE', #7159, #2214, #1358, .T. ) ;
#5282 = CIRCLE ( 'NONE', #3797, 4.999999999999997335 ) ;
#5283 = ORIENTED_EDGE ( 'NONE', *, *, #7636, .T. ) ;
#5284 = FACE_OUTER_BOUND ( 'NONE', #2206, .T. ) ;
#5285 = CARTESIAN_POINT ( 'NONE',  ( 0.000000000000000000, 0.000000000000000000, -250.0000000000000000 ) ) ;
#5286 = FACE_BOUND ( 'NONE', #7760, .T. ) ;
#5287 = DIRECTION ( 'NONE',  ( -0.000000000000000000, -0.000000000000000000, 1.000000000000000000 ) ) ;
#5288 = DIRECTION ( 'NONE',  ( -0.000000000000000000, -1.000000000000000000, -0.000000000000000000 ) ) ;
#5289 = FACE_BOUND ( 'NONE', #2346, .T. ) ;
#5290 = CARTESIAN_POINT ( 'NONE',  ( 75.00000000000000000, 0.000000000000000000, 12.50000000000000000 ) ) ;
#5291 = CARTESIAN_POINT ( 'NONE',  ( -105.0000000000000000, 72.49999999999997158, 19.99999999999998934 ) ) ;
#5292 = DIRECTION ( 'NONE',  ( -0.000000000000000000, -0.000000000000000000, 1.000000000000000000 ) ) ;
#5293 = VERTEX_POINT ( 'NONE', #4841 ) ;
#5294 = DIRECTION ( 'NONE',  ( 1.000000000000000000, 0.000000000000000000, -0.000000000000000000 ) ) ;
#5295 = DIRECTION ( 'NONE',  ( 1.224646799147348523E-16, 3.160065852750576588E-30, -1.000000000000000000 ) ) ;
#5296 = ORIENTED_EDGE ( 'NONE', *, *, #7340, .F. ) ;
#5297 = CIRCLE ( 'NONE', #3127, 54.99999999999995026 ) ;
#5298 = FACE_BOUND ( 'NONE', #7852, .T. ) ;
#5299 = CARTESIAN_POINT ( 'NONE',  ( 10.00000000000000000, -3.448762466456902719E-14, 93.74999999999998579 ) ) ;
#5300 = DIRECTION ( 'NONE',  ( 0.000000000000000000, 0.000000000000000000, -1.000000000000000000 ) ) ;
#5301 = CIRCLE ( 'NONE', #2858, 4.999999999999997335 ) ;
#5302 = ORIENTED_EDGE ( 'NONE', *, *, #2868, .F. ) ;
#5303 = LINE ( 'NONE', #4575, #7801 ) ;
#5304 = EDGE_LOOP ( 'NONE', ( #7488, #970, #1916, #2139, #4445 ) ) ;
#5305 = EDGE_CURVE ( 'NONE', #1946, #1562, #8134, .T. ) ;
#5306 = ADVANCED_FACE ( 'NONE', ( #3017 ), #6701, .F. ) ;
#5307 = CARTESIAN_POINT ( 'NONE',  ( -10.00000000000000000, -3.448762466456902719E-14, 93.74999999999998579 ) ) ;
#5308 = ORIENTED_EDGE ( 'NONE', *, *, #3547, .T. ) ;
#5309 = VERTEX_POINT ( 'NONE', #926 ) ;
#5310 = LINE ( 'NONE', #3952, #8346 ) ;
#5311 = DIRECTION ( 'NONE',  ( 1.000000000000000000, 0.000000000000000000, 0.000000000000000000 ) ) ;
#5312 = CARTESIAN_POINT ( 'NONE',  ( 60.99999999999998579, 55.00000000000000711, 27.50000000000000000 ) ) ;
#5313 = CIRCLE ( 'NONE', #5033, 8.999999999999994671 ) ;
#5314 = EDGE_CURVE ( 'NONE', #2083, #758, #6872, .T. ) ;
#5315 = VERTEX_POINT ( 'NONE', #2935 ) ;
#5316 = FACE_OUTER_BOUND ( 'NONE', #2231, .T. ) ;
#5317 = EDGE_LOOP ( 'NONE', ( #7079, #2592, #4144, #96 ) ) ;
#5318 = DIRECTION ( 'NONE',  ( 0.000000000000000000, 0.000000000000000000, -1.000000000000000000 ) ) ;
#5319 = VECTOR ( 'NONE', #5198, 1000.000000000000000 ) ;
#5320 = LINE ( 'NONE', #6021, #8323 ) ;
#5321 = DIRECTION ( 'NONE',  ( -1.752490724247359037E-17, 1.000000000000000000, 3.853078496550133260E-17 ) ) ;
#5322 = AXIS2_PLACEMENT_3D ( 'NONE', #4771, #7235, #6644 ) ;
#5323 = EDGE_CURVE ( 'NONE', #7049, #6111, #5438, .T. ) ;
#5324 = PRODUCT ( 'Probe', 'Probe', '', ( #4324 ) ) ;
#5325 = FACE_OUTER_BOUND ( 'NONE', #1747, .T. ) ;
#5326 = CARTESIAN_POINT ( 'NONE',  ( 10.00000000000000000, 2.291769404546313661E-14, -93.74999999999998579 ) ) ;
#5327 = CARTESIAN_POINT ( 'NONE',  ( 0.000000000000000000, 52.49999999999997868, 66.99999999999994316 ) ) ;
#5328 = LINE ( 'NONE', #7911, #4294 ) ;
#5329 = EDGE_LOOP ( 'NONE', ( #4860, #6097, #2996, #668 ) ) ;
#5330 = LINE ( 'NONE', #857, #6413 ) ;
#5331 = DIRECTION ( 'NONE',  ( 1.000000000000000000, 0.000000000000000000, 0.000000000000000000 ) ) ;
#5332 = CARTESIAN_POINT ( 'NONE',  ( 15.00000000000000000, 0.000000000000000000, -128.0000000000000284 ) ) ;
#5333 = DIRECTION ( 'NONE',  ( 1.000000000000000000, 0.000000000000000000, 0.000000000000000000 ) ) ;
#5334 = CARTESIAN_POINT ( 'NONE',  ( 0.000000000000000000, -15.00000000000000000, -126.0000000000000284 ) ) ;
#5335 = DIRECTION ( 'NONE',  ( 1.000000000000000000, 0.000000000000000000, 0.000000000000000000 ) ) ;
#5336 = CIRCLE ( 'NONE', #4516, 5.999999999999991118 ) ;
#5337 = DIRECTION ( 'NONE',  ( 1.000000000000000000, 0.000000000000000000, 0.000000000000000000 ) ) ;
#5338 = VERTEX_POINT ( 'NONE', #6061 ) ;
#5339 = FACE_OUTER_BOUND ( 'NONE', #7399, .T. ) ;
#5340 = CARTESIAN_POINT ( 'NONE',  ( 17.61817604250836311, 4.500000000000000000, -128.0000000000000284 ) ) ;
#5341 = ORIENTED_EDGE ( 'NONE', *, *, #3484, .F. ) ;
#5342 = VECTOR ( 'NONE', #6553, 1000.000000000000000 ) ;
#5343 = VERTEX_POINT ( 'NONE', #6231 ) ;
#5344 = CARTESIAN_POINT ( 'NONE',  ( -125.0000000000000000, 125.0000000000000568, -9.184850993605156622E-15 ) ) ;
#5345 = DIRECTION ( 'NONE',  ( 0.000000000000000000, 1.460819769243626884E-16, -1.000000000000000000 ) ) ;
#5346 = EDGE_CURVE ( 'NONE', #7256, #7568, #5644, .T. ) ;
#5347 = LINE ( 'NONE', #2284, #3694 ) ;
#5348 = DIRECTION ( 'NONE',  ( -0.000000000000000000, 0.8660254037844395958, 0.4999999999999985012 ) ) ;
#5349 = EDGE_LOOP ( 'NONE', ( #4189, #7875, #5813, #2244 ) ) ;
#5350 = ORIENTED_EDGE ( 'NONE', *, *, #2640, .F. ) ;
#5351 = DIRECTION ( 'NONE',  ( 1.000000000000000000, 0.000000000000000000, 0.000000000000000000 ) ) ;
#5352 = VERTEX_POINT ( 'NONE', #4271 ) ;
#5353 = VECTOR ( 'NONE', #4131, 1000.000000000000114 ) ;
#5354 = EDGE_CURVE ( 'NONE', #5384, #6772, #359, .T. ) ;
#5355 = EDGE_CURVE ( 'NONE', #3934, #5497, #6718, .T. ) ;
#5356 = AXIS2_PLACEMENT_3D ( 'NONE', #2240, #5383, #869 ) ;
#5357 = DIRECTION ( 'NONE',  ( -0.000000000000000000, -0.000000000000000000, 1.000000000000000000 ) ) ;
#5358 = AXIS2_PLACEMENT_3D ( 'NONE', #5360, #5405, #4080 ) ;
#5359 = CARTESIAN_POINT ( 'NONE',  ( 10.00000000000000000, 2.291769404546313661E-14, -93.74999999999998579 ) ) ;
#5360 = CARTESIAN_POINT ( 'NONE',  ( -109.4999999999999858, 114.9999999999999858, 10.00000000000000000 ) ) ;
#5361 = CARTESIAN_POINT ( 'NONE',  ( 0.000000000000000000, -72.49999999999998579, 79.99999999999995737 ) ) ;
#5362 = VECTOR ( 'NONE', #5391, 1000.000000000000000 ) ;
#5363 = DIRECTION ( 'NONE',  ( 0.000000000000000000, -0.000000000000000000, -1.000000000000000000 ) ) ;
#5364 = FACE_BOUND ( 'NONE', #2270, .T. ) ;
#5365 = CYLINDRICAL_SURFACE ( 'NONE', #5121, 5.999999999999991118 ) ;
#5366 = ORIENTED_EDGE ( 'NONE', *, *, #5100, .F. ) ;
#5367 = CARTESIAN_POINT ( 'NONE',  ( 5.000000000000000000, -2.342598717236898054, 4.057500000000003659 ) ) ;
#5368 = ADVANCED_FACE ( 'NONE', ( #971 ), #4792, .F. ) ;
#5369 = AXIS2_PLACEMENT_3D ( 'NONE', #4374, #7699, #3119 ) ;
#5370 = AXIS2_PLACEMENT_3D ( 'NONE', #6674, #3968, #894 ) ;
#5371 = ORIENTED_EDGE ( 'NONE', *, *, #7000, .T. ) ;
#5372 = ORIENTED_EDGE ( 'NONE', *, *, #8257, .T. ) ;
#5373 = FACE_OUTER_BOUND ( 'NONE', #2761, .T. ) ;
#5374 = CIRCLE ( 'NONE', #6447, 95.00000000000008527 ) ;
#5375 = VECTOR ( 'NONE', #7374, 1000.000000000000000 ) ;
#5376 = FACE_OUTER_BOUND ( 'NONE', #1013, .T. ) ;
#5377 = DIRECTION ( 'NONE',  ( -0.000000000000000000, -1.000000000000000000, -1.224646799147353207E-16 ) ) ;
#5378 = EDGE_CURVE ( 'NONE', #4856, #3986, #1603, .T. ) ;
#5379 = DIRECTION ( 'NONE',  ( 1.000000000000000000, 0.000000000000000000, 0.000000000000000000 ) ) ;
#5380 = SHAPE_REPRESENTATION_RELATIONSHIP ( 'NONE' , 'NONE' ,  #5477, #7858 ) ;
#5381 = CARTESIAN_POINT ( 'NONE',  ( -54.99999999999999289, 55.00000000000000711, 27.50000000000000000 ) ) ;
#5382 = AXIS2_PLACEMENT_3D ( 'NONE', #3325, #288, #1449 ) ;
#5383 = DIRECTION ( 'NONE',  ( -0.000000000000000000, 0.000000000000000000, 1.000000000000000000 ) ) ;
#5384 = VERTEX_POINT ( 'NONE', #3515 ) ;
#5385 = CARTESIAN_POINT ( 'NONE',  ( -115.0000000000000000, 115.0000000000000000, 20.00000000000000355 ) ) ;
#5386 = DIRECTION ( 'NONE',  ( -0.000000000000000000, -0.000000000000000000, 1.000000000000000000 ) ) ;
#5387 = VECTOR ( 'NONE', #7995, 1000.000000000000000 ) ;
#5388 = ORIENTED_EDGE ( 'NONE', *, *, #3036, .T. ) ;
#5389 = VERTEX_POINT ( 'NONE', #6142 ) ;
#5390 = DIRECTION ( 'NONE',  ( -1.000000000000000000, 0.000000000000000000, 0.000000000000000000 ) ) ;
#5391 = DIRECTION ( 'NONE',  ( -0.000000000000000000, -1.000000000000000000, 1.586032892321652236E-16 ) ) ;
#5392 = DIRECTION ( 'NONE',  ( 1.000000000000000000, 0.000000000000000000, 0.000000000000000000 ) ) ;
#5393 = DIRECTION ( 'NONE',  ( -1.000000000000000000, -0.000000000000000000, -0.000000000000000000 ) ) ;
#5394 = AXIS2_PLACEMENT_3D ( 'NONE', #206, #4969, #6923 ) ;
#5395 = VERTEX_POINT ( 'NONE', #4114 ) ;
#5396 = VERTEX_POINT ( 'NONE', #1050 ) ;
#5397 = CARTESIAN_POINT ( 'NONE',  ( 110.0000000000000142, 115.0000000000000000, 340.0000000000000000 ) ) ;
#5398 = EDGE_LOOP ( 'NONE', ( #5779, #358, #4464, #1637 ) ) ;
#5399 = CARTESIAN_POINT ( 'NONE',  ( 4.999999999999994671, 0.000000000000000000, 0.000000000000000000 ) ) ;
#5400 = ORIENTED_EDGE ( 'NONE', *, *, #3036, .F. ) ;
#5401 = LINE ( 'NONE', #2857, #7712 ) ;
#5402 = CARTESIAN_POINT ( 'NONE',  ( -115.0000000000000284, -115.0000000000000000, 20.00000000000000355 ) ) ;
#5403 = ADVANCED_FACE ( 'NONE', ( #2890, #8050 ), #5481, .F. ) ;
#5404 = EDGE_CURVE ( 'NONE', #4206, #8026, #2364, .T. ) ;
#5405 = DIRECTION ( 'NONE',  ( 0.000000000000000000, 0.000000000000000000, -1.000000000000000000 ) ) ;
#5406 = EDGE_CURVE ( 'NONE', #268, #5618, #1200, .T. ) ;
#5407 = CONICAL_SURFACE ( 'NONE', #5001, 5.999999999999991118, 1.029744258676652313 ) ;
#5408 = DIRECTION ( 'NONE',  ( 1.000000000000000000, 0.000000000000000000, 0.000000000000000000 ) ) ;
#5409 = CARTESIAN_POINT ( 'NONE',  ( 124.9999999999997442, -125.0000000000000000, 0.000000000000000000 ) ) ;
#5410 = CARTESIAN_POINT ( 'NONE',  ( -120.9999999999999005, -115.0000000000000000, 0.000000000000000000 ) ) ;
#5411 = CARTESIAN_POINT ( 'NONE',  ( -0.000000000000000000, 5.000000000000000000, 57.99999999999999289 ) ) ;
#5412 = ORIENTED_EDGE ( 'NONE', *, *, #2228, .T. ) ;
#5413 = VECTOR ( 'NONE', #7779, 1000.000000000000000 ) ;
#5414 = ORIENTED_EDGE ( 'NONE', *, *, #1980, .F. ) ;
#5415 = EDGE_CURVE ( 'NONE', #2791, #3078, #7402, .T. ) ;
#5416 = EDGE_CURVE ( 'NONE', #1836, #6640, #939, .T. ) ;
#5417 = DIRECTION ( 'NONE',  ( 1.000000000000000000, 0.000000000000000000, 0.000000000000000000 ) ) ;
#5418 = CARTESIAN_POINT ( 'NONE',  ( 95.00000000000001421, 1.163414459189985801E-14, 15.00000000000000000 ) ) ;
#5419 = CARTESIAN_POINT ( 'NONE',  ( -12.41960978562213924, -48.43326235599739249, -10.86247626165360636 ) ) ;
#5420 = DIRECTION ( 'NONE',  ( -1.000000000000000000, 0.000000000000000000, 0.000000000000000000 ) ) ;
#5421 = FACE_OUTER_BOUND ( 'NONE', #3023, .T. ) ;
#5422 = DIRECTION ( 'NONE',  ( 1.000000000000000000, 0.000000000000000000, 0.000000000000000000 ) ) ;
#5423 = CIRCLE ( 'NONE', #8115, 9.499999999999952038 ) ;
#5424 = ORIENTED_EDGE ( 'NONE', *, *, #5208, .F. ) ;
#5425 = CARTESIAN_POINT ( 'NONE',  ( 115.0000000000000000, 115.0000000000000000, 20.00000000000000355 ) ) ;
#5426 = EDGE_CURVE ( 'NONE', #323, #549, #1723, .T. ) ;
#5427 = APPLICATION_CONTEXT ( 'automotive_design' ) ;
#5428 = CARTESIAN_POINT ( 'NONE',  ( 2.775557561562893875E-14, -95.00000000000008527, 35.00000000000000000 ) ) ;
#5429 = ORIENTED_EDGE ( 'NONE', *, *, #8001, .F. ) ;
#5430 = ORIENTED_EDGE ( 'NONE', *, *, #767, .F. ) ;
#5431 = LINE ( 'NONE', #3783, #7272 ) ;
#5432 = DIRECTION ( 'NONE',  ( -0.000000000000000000, -0.000000000000000000, 1.000000000000000000 ) ) ;
#5433 = AXIS2_PLACEMENT_3D ( 'NONE', #3132, #5120, #4344 ) ;
#5434 = CARTESIAN_POINT ( 'NONE',  ( -125.0000000000000000, -52.50000000000000000, 190.0000000000000284 ) ) ;
#5435 = DIRECTION ( 'NONE',  ( 1.752490724247363967E-17, -1.000000000000000000, 3.853078496550152365E-17 ) ) ;
#5436 = VECTOR ( 'NONE', #7984, 1000.000000000000000 ) ;
#5437 = ORIENTED_EDGE ( 'NONE', *, *, #7172, .T. ) ;
#5438 = LINE ( 'NONE', #6747, #8343 ) ;
#5439 = VERTEX_POINT ( 'NONE', #1561 ) ;
#5440 = PLANE ( 'NONE',  #5786 ) ;
#5441 = CLOSED_SHELL ( 'NONE', ( #2548, #1393, #4936, #5672, #4886, #1209, #343, #862, #7373, #4460, #3497, #769 ) ) ;
#5442 = DIRECTION ( 'NONE',  ( 0.9992060621654691444, -0.03984024763698791605, 1.223674505719567166E-16 ) ) ;
#5443 = VERTEX_POINT ( 'NONE', #3188 ) ;
#5444 = LINE ( 'NONE', #7348, #3101 ) ;
#5445 = DIRECTION ( 'NONE',  ( 0.000000000000000000, -2.960594732333750610E-16, 1.000000000000000000 ) ) ;
#5446 = AXIS2_PLACEMENT_3D ( 'NONE', #2004, #7194, #1416 ) ;
#5447 = CARTESIAN_POINT ( 'NONE',  ( 0.000000000000000000, -4.685197434473809430, 7.372574772901430151E-15 ) ) ;
#5448 = PLANE ( 'NONE',  #457 ) ;
#5449 = CARTESIAN_POINT ( 'NONE',  ( -105.9999999999999858, 114.9999999999999858, 20.00000000000000000 ) ) ;
#5450 = LINE ( 'NONE', #4042, #803 ) ;
#5451 = EDGE_CURVE ( 'NONE', #1904, #3406, #5008, .T. ) ;
#5452 = ORIENTED_EDGE ( 'NONE', *, *, #6012, .T. ) ;
#5453 = B_SPLINE_CURVE_WITH_KNOTS ( 'NONE', 3,
 ( #281, #2944, #3611, #5534, #7978, #4923, #2896, #6707, #4760, #4235, #7393, #242, #2820, #936, #6754, #3520, #1058, #6103, #327, #5574, #3142, #2462, #5698, #2501, #3706, #1957, #551, #8190, #3118, #7650, #3194, #7005, #5098, #2581, #5055, #4495, #1781, #4971, #1865, #8322, #3798, #7606, #2418, #592, #3073, #7696, #5142, #7563, #1912, #8283 ),
 .UNSPECIFIED., .F., .F.,
 ( 4, 2, 2, 2, 2, 2, 2, 2, 2, 2, 2, 2, 2, 2, 2, 2, 2, 2, 2, 2, 2, 2, 2, 2, 4 ),
 ( 1.991839973943360954E-18, 0.002452303327911185479, 0.003678454991866776918, 0.004904606655822368357, 0.007356909983733552968, 0.008583061647689146575, 0.009809213311644738448, 0.01226151663955592219, 0.01348766830351151233, 0.01471381996746710420, 0.01593997163142269261, 0.01716612329537827927, 0.01961842662328945261, 0.02207072995120062595, 0.02452303327911179581, 0.02574918494306738595, 0.02697533660702297262, 0.02820148827097856276, 0.02942763993493414942, 0.03187994326284532970, 0.03310609492680091637, 0.03433224659075650997, 0.03678454991866769025, 0.03801070158262329080, 0.03923685324657887746 ),
 .UNSPECIFIED. ) ;
#5454 = ORIENTED_EDGE ( 'NONE', *, *, #461, .T. ) ;
#5455 = ADVANCED_FACE ( 'NONE', ( #1298 ), #7080, .F. ) ;
#5456 = PRESENTATION_LAYER_ASSIGNMENT (  '', '', ( #3014 ) ) ;
#5457 = ORIENTED_EDGE ( 'NONE', *, *, #443, .T. ) ;
#5458 = CARTESIAN_POINT ( 'NONE',  ( 115.0000000000000000, 115.0000000000000000, 340.0000000000000000 ) ) ;
#5459 = DIRECTION ( 'NONE',  ( 1.000000000000000000, 0.000000000000000000, 0.000000000000000000 ) ) ;
#5460 = EDGE_LOOP ( 'NONE', ( #6846, #4135 ) ) ;
#5461 =( LENGTH_UNIT ( ) NAMED_UNIT ( * ) SI_UNIT ( .MILLI., .METRE. ) );
#5462 = EDGE_CURVE ( 'NONE', #7568, #3934, #8315, .T. ) ;
#5463 = EDGE_CURVE ( 'NONE', #2791, #8231, #800, .T. ) ;
#5464 = DIRECTION ( 'NONE',  ( 0.000000000000000000, -1.000000000000000000, 0.000000000000000000 ) ) ;
#5465 = DIRECTION ( 'NONE',  ( -1.000000000000000000, -0.000000000000000000, -0.000000000000000000 ) ) ;
#5466 = EDGE_LOOP ( 'NONE', ( #1366, #1538, #4307, #8192 ) ) ;
#5467 = CARTESIAN_POINT ( 'NONE',  ( 4.999999999999994671, 0.000000000000000000, 0.000000000000000000 ) ) ;
#5468 = VECTOR ( 'NONE', #5379, 1000.000000000000000 ) ;
#5469 = CARTESIAN_POINT ( 'NONE',  ( 0.000000000000000000, -4.500000000000000000, -128.0000000000000284 ) ) ;
#5470 = ORIENTED_EDGE ( 'NONE', *, *, #6534, .F. ) ;
#5471 = DIRECTION ( 'NONE',  ( 1.000000000000000000, 0.000000000000000000, 0.000000000000000000 ) ) ;
#5472 = LINE ( 'NONE', #6092, #4544 ) ;
#5473 = AXIS2_PLACEMENT_3D ( 'NONE', #5684, #5082, #7765 ) ;
#5474 = PRESENTATION_STYLE_ASSIGNMENT (( #3978 ) ) ;
#5475 = EDGE_CURVE ( 'NONE', #4379, #6239, #7597, .T. ) ;
#5476 = DIRECTION ( 'NONE',  ( -0.000000000000000000, -0.000000000000000000, 1.000000000000000000 ) ) ;
#5477 = SHAPE_REPRESENTATION ( 'Probe head motor', ( #1299 ), #4925 ) ;
#5478 = ORIENTED_EDGE ( 'NONE', *, *, #6603, .F. ) ;
#5479 = CIRCLE ( 'NONE', #1848, 15.00000000000000178 ) ;
#5480 = VERTEX_POINT ( 'NONE', #1818 ) ;
#5481 = PLANE ( 'NONE',  #4142 ) ;
#5482 = AXIS2_PLACEMENT_3D ( 'NONE', #3688, #4957, #2318 ) ;
#5483 = ORIENTED_EDGE ( 'NONE', *, *, #3439, .T. ) ;
#5484 = DIRECTION ( 'NONE',  ( 1.000000000000000000, 1.321694076934710648E-16, 0.000000000000000000 ) ) ;
#5485 =( LENGTH_UNIT ( ) NAMED_UNIT ( * ) SI_UNIT ( .MILLI., .METRE. ) );
#5486 = CIRCLE ( 'NONE', #6419, 12.99999999999999822 ) ;
#5487 = ORIENTED_EDGE ( 'NONE', *, *, #2764, .F. ) ;
#5488 = CARTESIAN_POINT ( 'NONE',  ( 80.00000000000000000, 0.000000000000000000, 0.000000000000000000 ) ) ;
#5489 =( REPRESENTATION_RELATIONSHIP ('NONE','NONE', #6882, #573 ) REPRESENTATION_RELATIONSHIP_WITH_TRANSFORMATION ( #4887 )SHAPE_REPRESENTATION_RELATIONSHIP( ) );
#5490 = FACE_BOUND ( 'NONE', #234, .T. ) ;
#5491 = FACE_OUTER_BOUND ( 'NONE', #7684, .T. ) ;
#5492 = MECHANICAL_DESIGN_GEOMETRIC_PRESENTATION_REPRESENTATION (  '', ( #1309 ), #3587 ) ;
#5493 = AXIS2_PLACEMENT_3D ( 'NONE', #7326, #3457, #2274 ) ;
#5494 = ORIENTED_EDGE ( 'NONE', *, *, #5515, .F. ) ;
#5495 = SURFACE_STYLE_FILL_AREA ( #291 ) ;
#5496 = ORIENTED_EDGE ( 'NONE', *, *, #198, .T. ) ;
#5497 = VERTEX_POINT ( 'NONE', #7733 ) ;
#5498 = VECTOR ( 'NONE', #8333, 1000.000000000000000 ) ;
#5499 = ORIENTED_EDGE ( 'NONE', *, *, #5930, .F. ) ;
#5500 = AXIS2_PLACEMENT_3D ( 'NONE', #5548, #4136, #957 ) ;
#5501 = DIRECTION ( 'NONE',  ( 1.000000000000000000, 0.000000000000000000, 0.000000000000000000 ) ) ;
#5502 = CARTESIAN_POINT ( 'NONE',  ( 0.000000000000000000, 0.000000000000000000, -128.0000000000000284 ) ) ;
#5503 = ADVANCED_FACE ( 'NONE', ( #3744 ), #3228, .F. ) ;
#5504 = AXIS2_PLACEMENT_3D ( 'NONE', #5899, #2126, #2166 ) ;
#5505 = LINE ( 'NONE', #6079, #4708 ) ;
#5506 = ORIENTED_EDGE ( 'NONE', *, *, #1015, .F. ) ;
#5507 = SURFACE_STYLE_FILL_AREA ( #4214 ) ;
#5508 = VECTOR ( 'NONE', #73, 1000.000000000000000 ) ;
#5509 = DIRECTION ( 'NONE',  ( -0.000000000000000000, -1.000000000000000000, 1.586032892321652236E-16 ) ) ;
#5510 = VERTEX_POINT ( 'NONE', #7040 ) ;
#5511 = CIRCLE ( 'NONE', #2937, 5.999999999999991118 ) ;
#5512 = PLANE ( 'NONE',  #4615 ) ;
#5513 = CYLINDRICAL_SURFACE ( 'NONE', #350, 5.999999999999991118 ) ;
#5514 = EDGE_CURVE ( 'NONE', #7231, #2252, #6586, .T. ) ;
#5515 = EDGE_CURVE ( 'NONE', #6267, #2287, #8218, .T. ) ;
#5516 = LINE ( 'NONE', #6771, #6724 ) ;
#5517 = ORIENTED_EDGE ( 'NONE', *, *, #1245, .F. ) ;
#5518 = FACE_OUTER_BOUND ( 'NONE', #2326, .T. ) ;
#5519 = CARTESIAN_POINT ( 'NONE',  ( 95.00000000000008527, 0.000000000000000000, 20.00000000000000355 ) ) ;
#5520 = CIRCLE ( 'NONE', #383, 15.00000000000000000 ) ;
#5521 = EDGE_LOOP ( 'NONE', ( #3009, #5283, #2970, #2419 ) ) ;
#5522 = FACE_BOUND ( 'NONE', #3621, .T. ) ;
#5523 = VECTOR ( 'NONE', #6895, 1000.000000000000000 ) ;
#5524 = CIRCLE ( 'NONE', #6604, 3.000000000000002665 ) ;
#5525 = EDGE_LOOP ( 'NONE', ( #3147, #1069, #4191, #182, #856, #6799 ) ) ;
#5526 = EDGE_LOOP ( 'NONE', ( #651, #4062, #6993, #4140 ) ) ;
#5527 = CARTESIAN_POINT ( 'NONE',  ( 125.0000000000000000, 125.0000000000000000, 20.00000000000000000 ) ) ;
#5528 = ADVANCED_BREP_SHAPE_REPRESENTATION ( '', ( #950, #1299 ), #3819 ) ;
#5529 = ORIENTED_EDGE ( 'NONE', *, *, #5028, .F. ) ;
#5530 = PLANE ( 'NONE',  #2936 ) ;
#5531 = PRODUCT_CONTEXT ( 'NONE', #6285, 'mechanical' ) ;
#5532 = CIRCLE ( 'NONE', #4161, 8.000000000000000000 ) ;
#5533 = VERTEX_POINT ( 'NONE', #5691 ) ;
#5534 = CARTESIAN_POINT ( 'NONE',  ( 2.846087801003402529, 49.92054308009031161, -0.3214687869884013671 ) ) ;
#5535 = DIRECTION ( 'NONE',  ( 0.000000000000000000, 1.000000000000000000, -0.000000000000000000 ) ) ;
#5536 = PRODUCT_DEFINITION_SHAPE ( 'NONE', 'NONE',  #7576 ) ;
#5537 = EDGE_CURVE ( 'NONE', #1211, #5443, #2534, .T. ) ;
#5538 = CARTESIAN_POINT ( 'NONE',  ( -108.9999999999999147, -115.0000000000000000, 0.000000000000000000 ) ) ;
#5539 = VERTEX_POINT ( 'NONE', #1950 ) ;
#5540 = DIRECTION ( 'NONE',  ( 1.000000000000000000, 0.000000000000000000, 0.000000000000000000 ) ) ;
#5541 = VERTEX_POINT ( 'NONE', #3830 ) ;
#5542 = ORIENTED_EDGE ( 'NONE', *, *, #6013, .F. ) ;
#5543 = CIRCLE ( 'NONE', #2967, 75.00000000000001421 ) ;
#5544 = ORIENTED_EDGE ( 'NONE', *, *, #4523, .T. ) ;
#5545 = DIRECTION ( 'NONE',  ( 0.000000000000000000, 0.000000000000000000, 1.000000000000000000 ) ) ;
#5546 = DIRECTION ( 'NONE',  ( 0.000000000000000000, 0.000000000000000000, 1.000000000000000000 ) ) ;
#5547 = ORIENTED_EDGE ( 'NONE', *, *, #385, .F. ) ;
#5548 = CARTESIAN_POINT ( 'NONE',  ( 10.00000000000000000, 2.291769404546313661E-14, -93.74999999999998579 ) ) ;
#5549 = VECTOR ( 'NONE', #3955, 1000.000000000000000 ) ;
#5550 =( LENGTH_UNIT ( ) NAMED_UNIT ( * ) SI_UNIT ( .MILLI., .METRE. ) );
#5551 = EDGE_LOOP ( 'NONE', ( #6960, #4581 ) ) ;
#5552 = CARTESIAN_POINT ( 'NONE',  ( -54.99999999999999289, 75.00000000000000000, 27.50000000000000000 ) ) ;
#5553 = LINE ( 'NONE', #3102, #3865 ) ;
#5554 = CYLINDRICAL_SURFACE ( 'NONE', #4966, 54.99999999999996447 ) ;
#5555 = FACE_OUTER_BOUND ( 'NONE', #5701, .T. ) ;
#5556 = ORIENTED_EDGE ( 'NONE', *, *, #1968, .F. ) ;
#5557 = CARTESIAN_POINT ( 'NONE',  ( 115.0000000000000000, 115.0000000000000000, 270.0000000000000000 ) ) ;
#5558 = FACE_OUTER_BOUND ( 'NONE', #7124, .T. ) ;
#5559 = CARTESIAN_POINT ( 'NONE',  ( 5.000000000000000000, 3.513898075855358627, -2.028750000000004938 ) ) ;
#5560 = CIRCLE ( 'NONE', #2337, 20.00000000000000355 ) ;
#5561 = CARTESIAN_POINT ( 'NONE',  ( 95.00000000000002842, -95.00000000000002842, 70.00000000000000000 ) ) ;
#5562 = EDGE_CURVE ( 'NONE', #6622, #1581, #2409, .T. ) ;
#5563 = EDGE_CURVE ( 'NONE', #351, #3530, #586, .T. ) ;
#5564 = CARTESIAN_POINT ( 'NONE',  ( 125.0000000000000000, -52.50000000000000000, 190.0000000000000284 ) ) ;
#5565 = CIRCLE ( 'NONE', #7872, 4.999999999999990230 ) ;
#5566 = EDGE_LOOP ( 'NONE', ( #1870, #1376, #1329 ) ) ;
#5567 = CARTESIAN_POINT ( 'NONE',  ( 0.000000000000000000, 0.000000000000000000, 0.000000000000000000 ) ) ;
#5568 = ORIENTED_EDGE ( 'NONE', *, *, #4785, .T. ) ;
#5569 = AXIS2_PLACEMENT_3D ( 'NONE', #3481, #7796, #4160 ) ;
#5570 = DIRECTION ( 'NONE',  ( 0.000000000000000000, 1.000000000000000000, -0.000000000000000000 ) ) ;
#5571 = DIRECTION ( 'NONE',  ( 0.000000000000000000, 0.000000000000000000, 1.000000000000000000 ) ) ;
#5572 = EDGE_LOOP ( 'NONE', ( #4447, #3828, #3381, #2786 ) ) ;
#5573 = ORIENTED_EDGE ( 'NONE', *, *, #76, .F. ) ;
#5574 = CARTESIAN_POINT ( 'NONE',  ( 11.69960264931230043, 48.61219013327713157, -8.080179916824185682 ) ) ;
#5575 = EDGE_CURVE ( 'NONE', #4086, #5749, #5511, .T. ) ;
#5576 = ORIENTED_EDGE ( 'NONE', *, *, #5918, .T. ) ;
#5577 = LINE ( 'NONE', #8021, #5235 ) ;
#5578 = ORIENTED_EDGE ( 'NONE', *, *, #1026, .T. ) ;
#5579 = DIRECTION ( 'NONE',  ( 0.000000000000000000, 0.000000000000000000, -1.000000000000000000 ) ) ;
#5580 = CIRCLE ( 'NONE', #447, 54.99999999999995026 ) ;
#5581 = DIRECTION ( 'NONE',  ( 1.000000000000000000, 0.000000000000000000, 0.000000000000000000 ) ) ;
#5582 = LINE ( 'NONE', #3872, #923 ) ;
#5583 = ORIENTED_EDGE ( 'NONE', *, *, #6113, .T. ) ;
#5584 = VERTEX_POINT ( 'NONE', #5091 ) ;
#5585 = EDGE_CURVE ( 'NONE', #2918, #6076, #6997, .T. ) ;
#5586 = VERTEX_POINT ( 'NONE', #7685 ) ;
#5587 = CARTESIAN_POINT ( 'NONE',  ( -125.0000000000000000, -125.0000000000000000, -28.00000000000002487 ) ) ;
#5588 = CARTESIAN_POINT ( 'NONE',  ( -10.00000000000000000, 54.99999999999997158, -93.74999999999998579 ) ) ;
#5589 = CARTESIAN_POINT ( 'NONE',  ( 0.000000000000000000, 0.000000000000000000, 15.00000000000000000 ) ) ;
#5590 = VECTOR ( 'NONE', #4616, 1000.000000000000000 ) ;
#5591 = ORIENTED_EDGE ( 'NONE', *, *, #6012, .F. ) ;
#5592 = CARTESIAN_POINT ( 'NONE',  ( -1.644392415218294268, -49.97938897499117417, -0.08173415109641084253 ) ) ;
#5593 = ORIENTED_EDGE ( 'NONE', *, *, #1359, .T. ) ;
#5594 = ORIENTED_EDGE ( 'NONE', *, *, #1208, .T. ) ;
#5595 = DIRECTION ( 'NONE',  ( 0.000000000000000000, 1.224646799147353207E-16, 1.000000000000000000 ) ) ;
#5596 = CARTESIAN_POINT ( 'NONE',  ( 0.000000000000000000, -52.49999999999996447, 66.99999999999995737 ) ) ;
#5597 = CARTESIAN_POINT ( 'NONE',  ( 10.00000000000000000, -3.448762466456902719E-14, 93.74999999999998579 ) ) ;
#5598 = ORIENTED_EDGE ( 'NONE', *, *, #949, .F. ) ;
#5599 = CARTESIAN_POINT ( 'NONE',  ( 6.123233995736765296E-15, -49.99999999999998579, -100.0000000000000000 ) ) ;
#5600 = CARTESIAN_POINT ( 'NONE',  ( -114.9999999999999147, -115.0000000000000000, 0.000000000000000000 ) ) ;
#5601 = DIRECTION ( 'NONE',  ( -1.000000000000000000, -0.000000000000000000, 0.000000000000000000 ) ) ;
#5602 = CARTESIAN_POINT ( 'NONE',  ( 0.000000000000000000, 0.000000000000000000, 35.00000000000000000 ) ) ;
#5603 = VERTEX_POINT ( 'NONE', #4448 ) ;
#5604 = CARTESIAN_POINT ( 'NONE',  ( 0.000000000000000000, -4.685197434473809430, 7.372574772901430151E-15 ) ) ;
#5605 = CARTESIAN_POINT ( 'NONE',  ( 0.000000000000000000, 0.000000000000000000, 15.00000000000000000 ) ) ;
#5606 = ORIENTED_EDGE ( 'NONE', *, *, #1533, .F. ) ;
#5607 = EDGE_CURVE ( 'NONE', #1156, #1010, #6268, .T. ) ;
#5608 = LINE ( 'NONE', #8186, #4014 ) ;
#5609 = DIRECTION ( 'NONE',  ( 0.000000000000000000, -0.000000000000000000, -1.000000000000000000 ) ) ;
#5610 = VERTEX_POINT ( 'NONE', #4488 ) ;
#5611 = CONTEXT_DEPENDENT_SHAPE_REPRESENTATION ( #2219, #4990 ) ;
#5612 = DIRECTION ( 'NONE',  ( 1.000000000000000000, -0.000000000000000000, 0.000000000000000000 ) ) ;
#5613 = EDGE_LOOP ( 'NONE', ( #6810, #3659, #7090, #3492, #2052 ) ) ;
#5614 = CARTESIAN_POINT ( 'NONE',  ( 124.0000000000000000, -114.9999999999999716, 10.00000000000000000 ) ) ;
#5615 = AXIS2_PLACEMENT_3D ( 'NONE', #3785, #620, #5768 ) ;
#5616 = VERTEX_POINT ( 'NONE', #6436 ) ;
#5617 = DIRECTION ( 'NONE',  ( 0.000000000000000000, -0.000000000000000000, -1.000000000000000000 ) ) ;
#5618 = VERTEX_POINT ( 'NONE', #669 ) ;
#5619 = ORIENTED_EDGE ( 'NONE', *, *, #4100, .F. ) ;
#5620 = EDGE_CURVE ( 'NONE', #3934, #6145, #7556, .T. ) ;
#5621 = LINE ( 'NONE', #2992, #3221 ) ;
#5622 = EDGE_CURVE ( 'NONE', #3739, #4104, #244, .T. ) ;
#5623 = EDGE_CURVE ( 'NONE', #471, #8026, #141, .T. ) ;
#5624 = CARTESIAN_POINT ( 'NONE',  ( -121.0000000000000000, 115.0000000000000000, 20.00000000000000355 ) ) ;
#5625 = AXIS2_PLACEMENT_3D ( 'NONE', #823, #4560, #1373 ) ;
#5626 = VERTEX_POINT ( 'NONE', #7853 ) ;
#5627 = VERTEX_POINT ( 'NONE', #835 ) ;
#5628 = CARTESIAN_POINT ( 'NONE',  ( -99.99999999999991473, -115.0000000000000000, 250.0000000000000000 ) ) ;
#5629 = CARTESIAN_POINT ( 'NONE',  ( -75.00000000000000000, -75.00000000000000000, 27.50000000000000000 ) ) ;
#5630 = LINE ( 'NONE', #1796, #5523 ) ;
#5631 = ORIENTED_EDGE ( 'NONE', *, *, #2056, .F. ) ;
#5632 = CARTESIAN_POINT ( 'NONE',  ( 14.30908802125418511, -4.500000000000000000, -118.0000000000000284 ) ) ;
#5633 = AXIS2_PLACEMENT_3D ( 'NONE', #690, #5158, #1247 ) ;
#5634 = AXIS2_PLACEMENT_3D ( 'NONE', #7502, #7680, #1900 ) ;
#5635 = CARTESIAN_POINT ( 'NONE',  ( -1.110223024625156540E-13, -12.49999999999999645, 1.387778780781445676E-14 ) ) ;
#5636 = AXIS2_PLACEMENT_3D ( 'NONE', #6629, #7351, #5872 ) ;
#5637 = CARTESIAN_POINT ( 'NONE',  ( -31.74999999999995737, 0.000000000000000000, 0.000000000000000000 ) ) ;
#5638 = ADVANCED_FACE ( 'NONE', ( #2042 ), #4583, .F. ) ;
#5639 = AXIS2_PLACEMENT_3D ( 'NONE', #7084, #7737, #6934 ) ;
#5640 = EDGE_LOOP ( 'NONE', ( #3242, #6662, #6721, #6836 ) ) ;
#5641 = CARTESIAN_POINT ( 'NONE',  ( 125.0000000000000000, 125.0000000000000568, 19.99999999999998934 ) ) ;
#5642 = DIRECTION ( 'NONE',  ( 0.000000000000000000, 0.000000000000000000, -1.000000000000000000 ) ) ;
#5643 = EDGE_LOOP ( 'NONE', ( #3634, #2651, #8183, #5496 ) ) ;
#5644 = CIRCLE ( 'NONE', #2028, 9.499999999999952038 ) ;
#5645 = CARTESIAN_POINT ( 'NONE',  ( 125.0000000000000000, -125.0000000000000000, 340.0000000000000000 ) ) ;
#5646 = VERTEX_POINT ( 'NONE', #7926 ) ;
#5647 = CARTESIAN_POINT ( 'NONE',  ( 5.000000000000000000, 4.685197434473814759, -5.637851296924623057E-15 ) ) ;
#5648 = UNCERTAINTY_MEASURE_WITH_UNIT (LENGTH_MEASURE( 1.000000000000000082E-05 ), #2505, 'distance_accuracy_value', 'NONE');
#5649 = ORIENTED_EDGE ( 'NONE', *, *, #4348, .T. ) ;
#5650 = CARTESIAN_POINT ( 'NONE',  ( 0.000000000000000000, 115.0000000000000000, 250.0000000000000000 ) ) ;
#5651 = VECTOR ( 'NONE', #2202, 1000.000000000000000 ) ;
#5652 = FACE_OUTER_BOUND ( 'NONE', #8080, .T. ) ;
#5653 = AXIS2_PLACEMENT_3D ( 'NONE', #3699, #5815, #1264 ) ;
#5654 = EDGE_LOOP ( 'NONE', ( #8150, #636, #6202, #3229 ) ) ;
#5655 = CARTESIAN_POINT ( 'NONE',  ( -114.9999999999999716, 114.9999999999999858, 10.00000000000000000 ) ) ;
#5656 = CARTESIAN_POINT ( 'NONE',  ( 125.0000000000000000, 125.0000000000000568, -9.184850993605156622E-15 ) ) ;
#5657 = APPLICATION_PROTOCOL_DEFINITION ( 'draft international standard', 'automotive_design', 1998, #3212 ) ;
#5658 = EDGE_LOOP ( 'NONE', ( #6206, #8260, #4759 ) ) ;
#5659 = DIRECTION ( 'NONE',  ( -1.000000000000000000, 0.000000000000000000, 0.000000000000000000 ) ) ;
#5660 = AXIS2_PLACEMENT_3D ( 'NONE', #6263, #6987, #6312 ) ;
#5661 = AXIS2_PLACEMENT_3D ( 'NONE', #2784, #4005, #896 ) ;
#5662 = CARTESIAN_POINT ( 'NONE',  ( 10.00000000000000000, -3.448762466456902719E-14, 148.7499999999999432 ) ) ;
#5663 = CARTESIAN_POINT ( 'NONE',  ( 0.000000000000000000, 50.00000000000000000, 0.000000000000000000 ) ) ;
#5664 = DIRECTION ( 'NONE',  ( -0.000000000000000000, -0.000000000000000000, 1.000000000000000000 ) ) ;
#5665 = CIRCLE ( 'NONE', #4573, 12.99999999999999822 ) ;
#5666 = DIRECTION ( 'NONE',  ( 0.000000000000000000, -1.000000000000000000, 1.295896757998781966E-15 ) ) ;
#5667=STYLED_ITEM('',(#8386),#6502);
#5668 = ADVANCED_FACE ( 'NONE', ( #749 ), #7245, .F. ) ;
#5669 = CARTESIAN_POINT ( 'NONE',  ( -9.920332936303609017, 49.00669811220510752, -4.884022838024439039 ) ) ;
#5670 = VERTEX_POINT ( 'NONE', #6570 ) ;
#5671 = EDGE_CURVE ( 'NONE', #314, #2572, #7125, .T. ) ;
#5672 = ADVANCED_FACE ( 'NONE', ( #2724, #4025 ), #1387, .F. ) ;
#5673 = EDGE_LOOP ( 'NONE', ( #812, #2235, #4689, #5771 ) ) ;
#5674 = ADVANCED_FACE ( 'NONE', ( #1425 ), #7889, .F. ) ;
#5675 = DIRECTION ( 'NONE',  ( -0.000000000000000000, -0.000000000000000000, 1.000000000000000000 ) ) ;
#5676 = CARTESIAN_POINT ( 'NONE',  ( -105.0000000000000000, 105.0000000000000284, 340.0000000000000000 ) ) ;
#5677 = ORIENTED_EDGE ( 'NONE', *, *, #510, .F. ) ;
#5678 = CARTESIAN_POINT ( 'NONE',  ( -2.050159205374797455, -49.95957628852639942, -24.83755891087360013 ) ) ;
#5679 = EDGE_CURVE ( 'NONE', #986, #6306, #6448, .T. ) ;
#5680 = FACE_OUTER_BOUND ( 'NONE', #6190, .T. ) ;
#5681 = DIRECTION ( 'NONE',  ( 1.000000000000000000, 0.000000000000000000, 0.000000000000000000 ) ) ;
#5682 = FACE_OUTER_BOUND ( 'NONE', #1100, .T. ) ;
#5683 = CARTESIAN_POINT ( 'NONE',  ( 9.400408038818898859, -49.10908733398244408, -20.74923976180173213 ) ) ;
#5684 = CARTESIAN_POINT ( 'NONE',  ( 115.0000000000000000, 115.0000000000000000, 20.00000000000000355 ) ) ;
#5685 = CARTESIAN_POINT ( 'NONE',  ( 114.9999999999999147, 0.000000000000000000, 250.0000000000000000 ) ) ;
#5686 = ADVANCED_FACE ( 'NONE', ( #2082 ), #3984, .F. ) ;
#5687 = ORIENTED_EDGE ( 'NONE', *, *, #3651, .T. ) ;
#5688 = EDGE_CURVE ( 'NONE', #952, #469, #100, .T. ) ;
#5689 = DIRECTION ( 'NONE',  ( -1.000000000000000000, -0.000000000000000000, -0.000000000000000000 ) ) ;
#5690 = ORIENTED_EDGE ( 'NONE', *, *, #3764, .F. ) ;
#5691 = CARTESIAN_POINT ( 'NONE',  ( 75.00000000000000000, -54.99999999999999289, 27.50000000000000000 ) ) ;
#5692 = FACE_BOUND ( 'NONE', #5861, .T. ) ;
#5693 = ORIENTED_EDGE ( 'NONE', *, *, #3628, .T. ) ;
#5694 = LINE ( 'NONE', #2576, #6585 ) ;
#5695 = DIRECTION ( 'NONE',  ( 0.000000000000000000, 0.000000000000000000, 1.000000000000000000 ) ) ;
#5696 = ORIENTED_EDGE ( 'NONE', *, *, #2335, .F. ) ;
#5697 = APPLICATION_PROTOCOL_DEFINITION ( 'draft international standard', 'automotive_design', 1998, #299 ) ;
#5698 = CARTESIAN_POINT ( 'NONE',  ( 12.17797428566710138, 48.49436920628651393, -9.651054563031580713 ) ) ;
#5699 = VERTEX_POINT ( 'NONE', #7205 ) ;
#5700 = DIRECTION ( 'NONE',  ( 0.000000000000000000, 0.000000000000000000, 1.000000000000000000 ) ) ;
#5701 = EDGE_LOOP ( 'NONE', ( #1398, #1724 ) ) ;
#5702 = LINE ( 'NONE', #1272, #6053 ) ;
#5703 = AXIS2_PLACEMENT_3D ( 'NONE', #8120, #4011, #5331 ) ;
#5704 = VERTEX_POINT ( 'NONE', #5854 ) ;
#5705 = CARTESIAN_POINT ( 'NONE',  ( -12.47905948369886353, 48.41771210405730130, -13.33173448961933794 ) ) ;
#5706 = ORIENTED_EDGE ( 'NONE', *, *, #1976, .T. ) ;
#5707 = CARTESIAN_POINT ( 'NONE',  ( 0.000000000000000000, 0.000000000000000000, -120.5000000000000284 ) ) ;
#5708 = ORIENTED_EDGE ( 'NONE', *, *, #8258, .T. ) ;
#5709 = PLANE ( 'NONE',  #858 ) ;
#5710 = DIRECTION ( 'NONE',  ( -0.000000000000000000, -0.000000000000000000, 1.000000000000000000 ) ) ;
#5711 = AXIS2_PLACEMENT_3D ( 'NONE', #5641, #1289, #3176 ) ;
#5712 = DIRECTION ( 'NONE',  ( -0.000000000000000000, 0.000000000000000000, 1.000000000000000000 ) ) ;
#5713 = EDGE_CURVE ( 'NONE', #334, #4021, #4015, .T. ) ;
#5714 = ORIENTED_EDGE ( 'NONE', *, *, #1804, .F. ) ;
#5715 = PLANE ( 'NONE',  #2653 ) ;
#5716 = EDGE_CURVE ( 'NONE', #2612, #7451, #4530, .T. ) ;
#5717 = CLOSED_SHELL ( 'NONE', ( #6538, #3232, #757, #7268, #7956, #6218, #1284, #6217, #6001, #4949, #562, #5863, #7015, #1305, #6063, #3103, #4309, #2381, #7267, #6334, #665, #2678, #6565, #7955, #5674, #7692, #6437 ) ) ;
#5718 = CARTESIAN_POINT ( 'NONE',  ( -120.4999999999999716, 114.9999999999999858, 20.00000000000000000 ) ) ;
#5719 = CARTESIAN_POINT ( 'NONE',  ( 0.000000000000000000, 0.000000000000000000, -126.0000000000000284 ) ) ;
#5720 = AXIS2_PLACEMENT_3D ( 'NONE', #7294, #221, #2245 ) ;
#5721 = CARTESIAN_POINT ( 'NONE',  ( 0.000000000000000000, 0.000000000000000000, 15.00000000000000000 ) ) ;
#5722 = ADVANCED_FACE ( 'NONE', ( #181 ), #2759, .F. ) ;
#5723 = DIRECTION ( 'NONE',  ( -1.752490724247359037E-17, 1.000000000000000000, 3.853078496550133260E-17 ) ) ;
#5724 = CARTESIAN_POINT ( 'NONE',  ( 0.000000000000000000, 7.945337353457666419E-16, -150.0000000000000000 ) ) ;
#5725 = AXIS2_PLACEMENT_3D ( 'NONE', #5968, #3500, #5335 ) ;
#5726 = DIRECTION ( 'NONE',  ( -1.000000000000000000, -0.000000000000000000, -0.000000000000000000 ) ) ;
#5727 = AXIS2_PLACEMENT_3D ( 'NONE', #3426, #228, #7337 ) ;
#5728 = EDGE_LOOP ( 'NONE', ( #1353, #1862 ) ) ;
#5729 = ORIENTED_EDGE ( 'NONE', *, *, #1966, .F. ) ;
#5730 = PRODUCT_DEFINITION_CONTEXT ( 'detailed design', #8017, 'design' ) ;
#5731 = EDGE_LOOP ( 'NONE', ( #6572, #1696, #7063, #7470 ) ) ;
#5732 = DIRECTION ( 'NONE',  ( 1.000000000000000000, 0.000000000000000000, 0.000000000000000000 ) ) ;
#5733=STYLED_ITEM('',(#8400),#931);
#5734 = ORIENTED_EDGE ( 'NONE', *, *, #7394, .F. ) ;
#5735 = FACE_OUTER_BOUND ( 'NONE', #1478, .T. ) ;
#5736 = EDGE_CURVE ( 'NONE', #5293, #6212, #3421, .T. ) ;
#5737 = DIRECTION ( 'NONE',  ( -1.000000000000000000, -0.000000000000000000, -0.000000000000000000 ) ) ;
#5738 = ITEM_DEFINED_TRANSFORMATION ( 'NONE', 'NONE', #5569,  #1299 ) ;
#5739 = EDGE_LOOP ( 'NONE', ( #2057, #6943, #5542, #3606 ) ) ;
#5740 = DIRECTION ( 'NONE',  ( 1.000000000000000000, 0.000000000000000000, 0.000000000000000000 ) ) ;
#5741 = PRODUCT_DEFINITION_SHAPE ( 'NONE', 'NONE',  #8360 ) ;
#5742 = CARTESIAN_POINT ( 'NONE',  ( 125.0000000000000000, 125.0000000000000000, 340.0000000000000000 ) ) ;
#5743 = ORIENTED_EDGE ( 'NONE', *, *, #1197, .T. ) ;
#5744 = LINE ( 'NONE', #1563, #4289 ) ;
#5745 = LINE ( 'NONE', #3204, #215 ) ;
#5746 = CIRCLE ( 'NONE', #2124, 4.999999999999990230 ) ;
#5747 = AXIS2_PLACEMENT_3D ( 'NONE', #1940, #1290, #11 ) ;
#5748 = LINE ( 'NONE', #7177, #3857 ) ;
#5749 = VERTEX_POINT ( 'NONE', #7773 ) ;
#5750 = CIRCLE ( 'NONE', #6556, 20.00000000000000355 ) ;
#5751 = LINE ( 'NONE', #1368, #5498 ) ;
#5752 = DIRECTION ( 'NONE',  ( -1.752490724247359037E-17, 1.000000000000000000, 3.853078496550133260E-17 ) ) ;
#5753 = AXIS2_PLACEMENT_3D ( 'NONE', #4301, #389, #6766 ) ;
#5754 = DIRECTION ( 'NONE',  ( -0.000000000000000000, -0.000000000000000000, -1.000000000000000000 ) ) ;
#5755 = ORIENTED_EDGE ( 'NONE', *, *, #7515, .T. ) ;
#5756 = CARTESIAN_POINT ( 'NONE',  ( -9.920587673301467291, -49.00664693364539914, -20.11565191071548142 ) ) ;
#5757 = CARTESIAN_POINT ( 'NONE',  ( 0.000000000000000000, 9.244463733058732095E-30, -362.0000000000000000 ) ) ;
#5758 = ORIENTED_EDGE ( 'NONE', *, *, #7906, .F. ) ;
#5759 = CIRCLE ( 'NONE', #2134, 5.999999999999991118 ) ;
#5760 = ORIENTED_EDGE ( 'NONE', *, *, #5354, .T. ) ;
#5761 = EDGE_CURVE ( 'NONE', #3972, #554, #5102, .T. ) ;
#5762 = ADVANCED_FACE ( 'NONE', ( #7815 ), #311, .T. ) ;
#5763 = DIRECTION ( 'NONE',  ( -0.000000000000000000, -0.000000000000000000, -1.000000000000000000 ) ) ;
#5764 = AXIS2_PLACEMENT_3D ( 'NONE', #7532, #6805, #8072 ) ;
#5765 = CARTESIAN_POINT ( 'NONE',  ( -110.0000000000000142, 115.0000000000000000, 340.0000000000000000 ) ) ;
#5766 = FACE_OUTER_BOUND ( 'NONE', #3581, .T. ) ;
#5767 = CARTESIAN_POINT ( 'NONE',  ( 7.631816331990286528, -49.41886753685898270, -22.43335506184081751 ) ) ;
#5768 = DIRECTION ( 'NONE',  ( 0.000000000000000000, 0.000000000000000000, -1.000000000000000000 ) ) ;
#5769 = AXIS2_PLACEMENT_3D ( 'NONE', #5685, #6390, #5045 ) ;
#5770 = PLANE ( 'NONE',  #5634 ) ;
#5771 = ORIENTED_EDGE ( 'NONE', *, *, #8302, .F. ) ;
#5772 = VECTOR ( 'NONE', #4414, 1000.000000000000000 ) ;
#5773 = ADVANCED_FACE ( 'NONE', ( #1592 ), #5554, .T. ) ;
#5774 = ADVANCED_FACE ( 'NONE', ( #4181 ), #8039, .F. ) ;
#5775 = VERTEX_POINT ( 'NONE', #3504 ) ;
#5776 = AXIS2_PLACEMENT_3D ( 'NONE', #1429, #2158, #145 ) ;
#5777 = VERTEX_POINT ( 'NONE', #2843 ) ;
#5778 = DIRECTION ( 'NONE',  ( 1.000000000000000000, 0.000000000000000000, 0.000000000000000000 ) ) ;
#5779 = ORIENTED_EDGE ( 'NONE', *, *, #3154, .T. ) ;
#5780 = DIRECTION ( 'NONE',  ( -0.000000000000000000, -0.000000000000000000, -1.000000000000000000 ) ) ;
#5781 = CARTESIAN_POINT ( 'NONE',  ( -115.0000000000000426, -115.0000000000000000, 16.39483628583463570 ) ) ;
#5782 = AXIS2_PLACEMENT_3D ( 'NONE', #4497, #1149, #5700 ) ;
#5783 = EDGE_LOOP ( 'NONE', ( #8065, #7347, #8049, #8012 ) ) ;
#5784 = CARTESIAN_POINT ( 'NONE',  ( 0.000000000000000000, 0.000000000000000000, 0.000000000000000000 ) ) ;
#5785 = ORIENTED_EDGE ( 'NONE', *, *, #4512, .T. ) ;
#5786 = AXIS2_PLACEMENT_3D ( 'NONE', #8235, #5166, #3794 ) ;
#5787 = CIRCLE ( 'NONE', #6175, 95.00000000000008527 ) ;
#5788 = CARTESIAN_POINT ( 'NONE',  ( 95.00000000000002842, -95.00000000000002842, 70.00000000000000000 ) ) ;
#5789 = CARTESIAN_POINT ( 'NONE',  ( 1.592040838891560279E-15, 72.49999999999995737, 92.99999999999994316 ) ) ;
#5790 = ORIENTED_EDGE ( 'NONE', *, *, #7751, .T. ) ;
#5791 = DIRECTION ( 'NONE',  ( 1.000000000000000000, 0.000000000000000000, 0.000000000000000000 ) ) ;
#5792 = CIRCLE ( 'NONE', #7687, 4.999999999999990230 ) ;
#5793 = CARTESIAN_POINT ( 'NONE',  ( 50.00000000000000000, 55.00000000000000000, 240.0000000000000284 ) ) ;
#5794 = ORIENTED_EDGE ( 'NONE', *, *, #8207, .F. ) ;
#5795 = EDGE_CURVE ( 'NONE', #5876, #4314, #5787, .T. ) ;
#5796 = EDGE_CURVE ( 'NONE', #6702, #7449, #266, .T. ) ;
#5797 = CARTESIAN_POINT ( 'NONE',  ( 0.000000000000000000, -72.49999999999997158, 20.00000000000001776 ) ) ;
#5798 = VECTOR ( 'NONE', #2911, 1000.000000000000000 ) ;
#5799 = MECHANICAL_DESIGN_GEOMETRIC_PRESENTATION_REPRESENTATION (  '', ( #5667 ), #541 ) ;
#5800 = DIRECTION ( 'NONE',  ( 0.000000000000000000, 0.000000000000000000, 1.000000000000000000 ) ) ;
#5801 = ORIENTED_EDGE ( 'NONE', *, *, #1448, .T. ) ;
#5802 = LINE ( 'NONE', #6300, #2131 ) ;
#5803 =( LENGTH_UNIT ( ) NAMED_UNIT ( * ) SI_UNIT ( .MILLI., .METRE. ) );
#5804 = AXIS2_PLACEMENT_3D ( 'NONE', #5139, #2497, #3233 ) ;
#5805 = ORIENTED_EDGE ( 'NONE', *, *, #5416, .T. ) ;
#5806 = ORIENTED_EDGE ( 'NONE', *, *, #2238, .F. ) ;
#5807 = DIRECTION ( 'NONE',  ( 1.000000000000000000, 0.000000000000000000, 0.000000000000000000 ) ) ;
#5808 = DIRECTION ( 'NONE',  ( 0.000000000000000000, -1.000000000000000000, 1.586032892321652236E-16 ) ) ;
#5809 = CARTESIAN_POINT ( 'NONE',  ( 8.256742446866514484, -49.31458024324042810, -3.106261761854192560 ) ) ;
#5810 = DIRECTION ( 'NONE',  ( -0.000000000000000000, -0.000000000000000000, -1.000000000000000000 ) ) ;
#5811 = DIRECTION ( 'NONE',  ( 0.000000000000000000, -1.000000000000000000, 0.000000000000000000 ) ) ;
#5812 = ORIENTED_EDGE ( 'NONE', *, *, #1189, .F. ) ;
#5813 = ORIENTED_EDGE ( 'NONE', *, *, #2105, .F. ) ;
#5814 = ORIENTED_EDGE ( 'NONE', *, *, #2517, .T. ) ;
#5815 = DIRECTION ( 'NONE',  ( -0.000000000000000000, -0.000000000000000000, 1.000000000000000000 ) ) ;
#5816 = ORIENTED_EDGE ( 'NONE', *, *, #5671, .F. ) ;
#5817 = CARTESIAN_POINT ( 'NONE',  ( 0.000000000000000000, 0.000000000000000000, 35.00000000000000000 ) ) ;
#5818 = DIRECTION ( 'NONE',  ( 6.106226635438364917E-16, 3.154042683594196846E-17, 1.000000000000000000 ) ) ;
#5819 = CARTESIAN_POINT ( 'NONE',  ( -105.0000000000000000, 105.0000000000000284, 340.0000000000000000 ) ) ;
#5820 = EDGE_CURVE ( 'NONE', #2665, #4485, #6814, .T. ) ;
#5821 = EDGE_CURVE ( 'NONE', #5539, #5396, #5516, .T. ) ;
#5822 = AXIS2_PLACEMENT_3D ( 'NONE', #6137, #1638, #2810 ) ;
#5823 = PLANE ( 'NONE',  #4454 ) ;
#5824 = EDGE_LOOP ( 'NONE', ( #6809, #7520 ) ) ;
#5825 = LINE ( 'NONE', #5742, #5772 ) ;
#5826 = VERTEX_POINT ( 'NONE', #8124 ) ;
#5827 = DIRECTION ( 'NONE',  ( 0.000000000000000000, 0.000000000000000000, 1.000000000000000000 ) ) ;
#5828 = EDGE_CURVE ( 'NONE', #7656, #4494, #6861, .T. ) ;
#5829 = EDGE_CURVE ( 'NONE', #3069, #5876, #1085, .T. ) ;
#5830 = CARTESIAN_POINT ( 'NONE',  ( 5.551115123125782702E-14, 12.50000000000001066, -1.387778780781445676E-14 ) ) ;
#5831 = CIRCLE ( 'NONE', #2849, 5.999999999999991118 ) ;
#5832 = LINE ( 'NONE', #5793, #6962 ) ;
#5833 = LINE ( 'NONE', #6342, #7526 ) ;
#5834 = DIRECTION ( 'NONE',  ( -0.000000000000000000, -0.000000000000000000, -1.000000000000000000 ) ) ;
#5835 = FACE_BOUND ( 'NONE', #7259, .T. ) ;
#5836 = VECTOR ( 'NONE', #2453, 1000.000000000000114 ) ;
#5837 = AXIS2_PLACEMENT_3D ( 'NONE', #2556, #7623, #1799 ) ;
#5838 = CARTESIAN_POINT ( 'NONE',  ( 14.30908802125418511, -4.500000000000000000, -126.0000000000000284 ) ) ;
#5839 = ORIENTED_EDGE ( 'NONE', *, *, #7163, .T. ) ;
#5840 = ADVANCED_FACE ( 'NONE', ( #7965 ), #3550, .T. ) ;
#5841 = CARTESIAN_POINT ( 'NONE',  ( -120.0000000000000000, -120.0000000000000000, -28.00000000000002487 ) ) ;
#5842 = CARTESIAN_POINT ( 'NONE',  ( 115.0000000000000000, -114.9999999999999147, 108.4000000000000341 ) ) ;
#5843 = ORIENTED_EDGE ( 'NONE', *, *, #5974, .F. ) ;
#5844 = DIRECTION ( 'NONE',  ( 1.000000000000000000, 0.000000000000000000, -0.000000000000000000 ) ) ;
#5845 = DIRECTION ( 'NONE',  ( 1.000000000000000000, 0.000000000000000000, 0.000000000000000000 ) ) ;
#5846 = DIRECTION ( 'NONE',  ( 1.000000000000000000, 0.000000000000000000, 0.000000000000000000 ) ) ;
#5847 = AXIS2_PLACEMENT_3D ( 'NONE', #4737, #7409, #1540 ) ;
#5848 = CARTESIAN_POINT ( 'NONE',  ( 11.85818221415417462, -48.57454970542615769, -8.462724116359982673 ) ) ;
#5849 = DIRECTION ( 'NONE',  ( 0.000000000000000000, 0.000000000000000000, -1.000000000000000000 ) ) ;
#5850 = DIRECTION ( 'NONE',  ( 1.000000000000000000, 0.000000000000000000, 0.000000000000000000 ) ) ;
#5851 = ORIENTED_EDGE ( 'NONE', *, *, #4417, .T. ) ;
#5852 = ORIENTED_EDGE ( 'NONE', *, *, #5463, .F. ) ;
#5853 = ORIENTED_EDGE ( 'NONE', *, *, #921, .T. ) ;
#5854 = CARTESIAN_POINT ( 'NONE',  ( 5.000000000000000000, -2.342598717236898054, 4.057500000000003659 ) ) ;
#5855 = VERTEX_POINT ( 'NONE', #4826 ) ;
#5856 = LINE ( 'NONE', #3424, #5651 ) ;
#5857 = DIRECTION ( 'NONE',  ( 0.000000000000000000, 0.000000000000000000, -1.000000000000000000 ) ) ;
#5858 = AXIS2_PLACEMENT_3D ( 'NONE', #344, #262, #6045 ) ;
#5859 = FACE_OUTER_BOUND ( 'NONE', #1201, .T. ) ;
#5860 = APPLICATION_CONTEXT ( 'automotive_design' ) ;
#5861 = EDGE_LOOP ( 'NONE', ( #1414, #7746 ) ) ;
#5862 = ORIENTED_EDGE ( 'NONE', *, *, #615, .T. ) ;
#5863 = ADVANCED_FACE ( 'NONE', ( #2356 ), #1611, .T. ) ;
#5864 = ORIENTED_EDGE ( 'NONE', *, *, #1976, .F. ) ;
#5865 = CARTESIAN_POINT ( 'NONE',  ( -10.00000000000000000, -54.99999999999995026, -93.75000000000001421 ) ) ;
#5866 = EDGE_LOOP ( 'NONE', ( #7425, #5049, #418, #3312 ) ) ;
#5867 = CARTESIAN_POINT ( 'NONE',  ( -115.0000000000000000, -115.0000000000000000, 340.0000000000000000 ) ) ;
#5868 = CARTESIAN_POINT ( 'NONE',  ( -3.256071768936462885, 49.89543388580307948, -0.4244881437574492544 ) ) ;
#5869 = DIRECTION ( 'NONE',  ( -0.000000000000000000, 0.000000000000000000, 1.000000000000000000 ) ) ;
#5870 = EDGE_CURVE ( 'NONE', #624, #5179, #525, .T. ) ;
#5871 = EDGE_CURVE ( 'NONE', #4377, #3745, #4831, .T. ) ;
#5872 = DIRECTION ( 'NONE',  ( -1.000000000000000000, 0.000000000000000000, 0.000000000000000000 ) ) ;
#5873 = DIRECTION ( 'NONE',  ( 0.000000000000000000, 0.000000000000000000, 1.000000000000000000 ) ) ;
#5874 = CIRCLE ( 'NONE', #7225, 37.49999999999999289 ) ;
#5875 = CARTESIAN_POINT ( 'NONE',  ( 0.000000000000000000, 0.000000000000000000, 20.00000000000000000 ) ) ;
#5876 = VERTEX_POINT ( 'NONE', #5428 ) ;
#5877 = FACE_OUTER_BOUND ( 'NONE', #7681, .T. ) ;
#5878 = DIRECTION ( 'NONE',  ( 1.000000000000000000, 3.155443620884047222E-30, 1.224646799147346798E-16 ) ) ;
#5879 = VERTEX_POINT ( 'NONE', #4101 ) ;
#5880=STYLED_ITEM('',(#8400),#3512);
#5881 = CARTESIAN_POINT ( 'NONE',  ( 0.000000000000000000, 2.499999999999996891, -150.0000000000000000 ) ) ;
#5882 = DIRECTION ( 'NONE',  ( -0.000000000000000000, -0.000000000000000000, 1.000000000000000000 ) ) ;
#5883 = DIRECTION ( 'NONE',  ( 1.000000000000000000, 0.000000000000000000, 0.000000000000000000 ) ) ;
#5884 = CARTESIAN_POINT ( 'NONE',  ( 0.000000000000000000, 0.000000000000000000, 0.000000000000000000 ) ) ;
#5885 = AXIS2_PLACEMENT_3D ( 'NONE', #722, #3985, #4463 ) ;
#5886 = DIRECTION ( 'NONE',  ( 1.000000000000000000, 0.000000000000000000, 0.000000000000000000 ) ) ;
#5887 = ORIENTED_EDGE ( 'NONE', *, *, #4563, .T. ) ;
#5888 = CARTESIAN_POINT ( 'NONE',  ( 102.5000000000000000, 0.000000000000000000, 0.000000000000000000 ) ) ;
#5889 = ADVANCED_FACE ( 'NONE', ( #8084 ), #2315, .F. ) ;
#5890 = AXIS2_PLACEMENT_3D ( 'NONE', #39, #3165, #4552 ) ;
#5891 = EDGE_LOOP ( 'NONE', ( #3704, #218, #8320, #634 ) ) ;
#5892 = CARTESIAN_POINT ( 'NONE',  ( 115.0000000000000000, 114.9999999999999716, 20.00000000000000000 ) ) ;
#5893 = VECTOR ( 'NONE', #6122, 1000.000000000000000 ) ;
#5894 = VERTEX_POINT ( 'NONE', #2802 ) ;
#5895 = DIRECTION ( 'NONE',  ( -0.000000000000000000, -1.000000000000000000, -0.000000000000000000 ) ) ;
#5896 = DIRECTION ( 'NONE',  ( -0.000000000000000000, -0.000000000000000000, 1.000000000000000000 ) ) ;
#5897 = VECTOR ( 'NONE', #5288, 1000.000000000000000 ) ;
#5898 = DIRECTION ( 'NONE',  ( 1.000000000000000000, 0.000000000000000000, 0.000000000000000000 ) ) ;
#5899 = CARTESIAN_POINT ( 'NONE',  ( 102.5000000000000000, 0.000000000000000000, 0.000000000000000000 ) ) ;
#5900 = AXIS2_PLACEMENT_3D ( 'NONE', #4716, #70, #2210 ) ;
#5901 = ORIENTED_EDGE ( 'NONE', *, *, #5563, .T. ) ;
#5902 = CARTESIAN_POINT ( 'NONE',  ( -121.0000000000000000, 115.0000000000000000, 70.00000000000000000 ) ) ;
#5903 = VECTOR ( 'NONE', #6719, 1000.000000000000000 ) ;
#5904 = EDGE_LOOP ( 'NONE', ( #2066, #388, #3100, #2435, #4931, #976, #1654, #340 ) ) ;
#5905 = CARTESIAN_POINT ( 'NONE',  ( -2.854599402353548587, 49.92007443197289263, -0.3233859435660823567 ) ) ;
#5906 = AXIS2_PLACEMENT_3D ( 'NONE', #3987, #62, #3268 ) ;
#5907 = AXIS2_PLACEMENT_3D ( 'NONE', #543, #3112, #6359 ) ;
#5908 = DIRECTION ( 'NONE',  ( -0.000000000000000000, -0.000000000000000000, -1.000000000000000000 ) ) ;
#5909 = VERTEX_POINT ( 'NONE', #4867 ) ;
#5910 = LINE ( 'NONE', #1489, #7672 ) ;
#5911 = DIRECTION ( 'NONE',  ( -1.000000000000000000, 0.000000000000000000, 0.000000000000000000 ) ) ;
#5912 = AXIS2_PLACEMENT_3D ( 'NONE', #3552, #7461, #6131 ) ;
#5913 = VECTOR ( 'NONE', #4063, 1000.000000000000000 ) ;
#5914 = DIRECTION ( 'NONE',  ( 0.000000000000000000, 0.4999999999999984457, -0.8660254037844394848 ) ) ;
#5915 = ORIENTED_EDGE ( 'NONE', *, *, #6709, .T. ) ;
#5916 = CARTESIAN_POINT ( 'NONE',  ( -120.0000000000000000, 125.0000000000000000, -28.00000000000002487 ) ) ;
#5917 = APPLICATION_PROTOCOL_DEFINITION ( 'draft international standard', 'automotive_design', 1998, #6720 ) ;
#5918 = EDGE_CURVE ( 'NONE', #4729, #14, #7414, .T. ) ;
#5919 = CARTESIAN_POINT ( 'NONE',  ( -115.0000000000000284, -115.0000000000000000, 70.00000000000000000 ) ) ;
#5920 = ADVANCED_FACE ( 'NONE', ( #1551 ), #4603, .F. ) ;
#5921 = ORIENTED_EDGE ( 'NONE', *, *, #5038, .T. ) ;
#5922 = CIRCLE ( 'NONE', #3219, 15.00000000000001421 ) ;
#5923 = VECTOR ( 'NONE', #162, 1000.000000000000000 ) ;
#5924 = DIRECTION ( 'NONE',  ( -0.000000000000000000, -0.000000000000000000, 1.000000000000000000 ) ) ;
#5925 = LINE ( 'NONE', #1659, #1446 ) ;
#5926 = LINE ( 'NONE', #133, #1750 ) ;
#5927 = DIRECTION ( 'NONE',  ( 1.000000000000000000, 0.000000000000000000, 0.000000000000000000 ) ) ;
#5928 = EDGE_CURVE ( 'NONE', #5510, #1156, #2433, .T. ) ;
#5929 = EDGE_CURVE ( 'NONE', #5186, #3530, #6904, .T. ) ;
#5930 = EDGE_CURVE ( 'NONE', #7972, #2241, #732, .T. ) ;
#5931 = AXIS2_PLACEMENT_3D ( 'NONE', #4847, #4196, #7437 ) ;
#5932 = CARTESIAN_POINT ( 'NONE',  ( 20.76917701662883076, 0.000000000000000000, 0.000000000000000000 ) ) ;
#5933 = ORIENTED_EDGE ( 'NONE', *, *, #7029, .F. ) ;
#5934 = DIRECTION ( 'NONE',  ( -0.000000000000000000, -0.000000000000000000, 1.000000000000000000 ) ) ;
#5935 = DIRECTION ( 'NONE',  ( -1.000000000000000000, 0.000000000000000000, -0.000000000000000000 ) ) ;
#5936 = ORIENTED_EDGE ( 'NONE', *, *, #3135, .F. ) ;
#5937 = VERTEX_POINT ( 'NONE', #2671 ) ;
#5938 = CARTESIAN_POINT ( 'NONE',  ( 1.592040838891559490E-15, 125.0000000000000568, 92.99999999999992895 ) ) ;
#5939 = DIRECTION ( 'NONE',  ( 0.000000000000000000, -0.000000000000000000, -1.000000000000000000 ) ) ;
#5940 = EDGE_CURVE ( 'NONE', #6702, #5539, #1893, .T. ) ;
#5941 = ADVANCED_FACE ( 'NONE', ( #4952, #7628, #2482, #1128, #5835, #3733 ), #5039, .F. ) ;
#5942 = CARTESIAN_POINT ( 'NONE',  ( -114.9999999999999147, 115.0000000000000000, 8.205133554287239938E-16 ) ) ;
#5943 = AXIS2_PLACEMENT_3D ( 'NONE', #8019, #4800, #2295 ) ;
#5944 = EDGE_CURVE ( 'NONE', #7524, #3696, #384, .T. ) ;
#5945 = FACE_OUTER_BOUND ( 'NONE', #3630, .T. ) ;
#5946 = ORIENTED_EDGE ( 'NONE', *, *, #3651, .F. ) ;
#5947 = CARTESIAN_POINT ( 'NONE',  ( 120.5000000000000000, -114.9999999999999716, 10.00000000000000000 ) ) ;
#5948 = AXIS2_PLACEMENT_3D ( 'NONE', #318, #5476, #2885 ) ;
#5949 = CARTESIAN_POINT ( 'NONE',  ( -55.00000000000000711, -55.00000000000000000, 216.9956969048622284 ) ) ;
#5950 = ORIENTED_EDGE ( 'NONE', *, *, #5796, .F. ) ;
#5951 = CARTESIAN_POINT ( 'NONE',  ( 0.000000000000000000, 0.000000000000000000, -27.50000000000000000 ) ) ;
#5952 = PLANE ( 'NONE',  #1958 ) ;
#5953 = LINE ( 'NONE', #4681, #229 ) ;
#5954 = CARTESIAN_POINT ( 'NONE',  ( 55.00000000000000711, -75.00000000000000000, 27.50000000000000000 ) ) ;
#5955 = CARTESIAN_POINT ( 'NONE',  ( -114.9999999999999147, 115.0000000000000000, 250.0000000000000000 ) ) ;
#5956 = DIRECTION ( 'NONE',  ( 0.000000000000000000, -1.000000000000000000, -1.224646799147353207E-16 ) ) ;
#5957 = CARTESIAN_POINT ( 'NONE',  ( 0.000000000000000000, 0.000000000000000000, -6.999999999999999112 ) ) ;
#5958 = AXIS2_PLACEMENT_3D ( 'NONE', #1947, #1384, #6524 ) ;
#5959 = DIRECTION ( 'NONE',  ( 1.000000000000000000, 0.000000000000000000, 0.000000000000000000 ) ) ;
#5960 = ORIENTED_EDGE ( 'NONE', *, *, #2585, .T. ) ;
#5961 = VECTOR ( 'NONE', #6839, 1000.000000000000000 ) ;
#5962 = CARTESIAN_POINT ( 'NONE',  ( 0.000000000000000000, 125.0000000000000000, -12.50000000000000000 ) ) ;
#5963 = DIRECTION ( 'NONE',  ( -1.000000000000000000, -0.000000000000000000, -0.000000000000000000 ) ) ;
#5964 = AXIS2_PLACEMENT_3D ( 'NONE', #1374, #4797, #6510 ) ;
#5965 = EDGE_CURVE ( 'NONE', #3065, #4671, #80, .T. ) ;
#5966 = CARTESIAN_POINT ( 'NONE',  ( 115.0000000000000000, 115.0000000000000000, 70.00000000000000000 ) ) ;
#5967 =( LENGTH_UNIT ( ) NAMED_UNIT ( * ) SI_UNIT ( .MILLI., .METRE. ) );
#5968 = CARTESIAN_POINT ( 'NONE',  ( -55.00000000000000000, 55.00000000000000000, 220.0000000000000284 ) ) ;
#5969 = CARTESIAN_POINT ( 'NONE',  ( 125.0000000000000000, -120.0000000000000000, -28.00000000000002487 ) ) ;
#5970 = FACE_BOUND ( 'NONE', #5460, .T. ) ;
#5971 = ORIENTED_EDGE ( 'NONE', *, *, #3277, .F. ) ;
#5972 = EDGE_CURVE ( 'NONE', #5396, #7449, #3092, .T. ) ;
#5973 = DIRECTION ( 'NONE',  ( 1.224646799147353207E-16, -1.000000000000000000, 0.000000000000000000 ) ) ;
#5974 = EDGE_CURVE ( 'NONE', #1281, #718, #671, .T. ) ;
#5975 = ORIENTED_EDGE ( 'NONE', *, *, #7055, .T. ) ;
#5976 = VERTEX_POINT ( 'NONE', #3890 ) ;
#5977 = FACE_BOUND ( 'NONE', #4810, .T. ) ;
#5978 = DIRECTION ( 'NONE',  ( -0.000000000000000000, -0.000000000000000000, -1.000000000000000000 ) ) ;
#5979 = DIRECTION ( 'NONE',  ( -1.000000000000000000, -0.000000000000000000, -0.000000000000000000 ) ) ;
#5980 = LINE ( 'NONE', #65, #7724 ) ;
#5981 = CLOSED_SHELL ( 'NONE', ( #7486, #3378, #7314, #3074, #3286, #4511, #7914, #7447, #6697, #1829, #4407, #2018, #6170, #1663, #617, #5250, #4687, #1075, #7218, #3295, #4835, #4246, #5889, #6200, #6167, #1498, #1930, #5196 ) ) ;
#5982 = ORIENTED_EDGE ( 'NONE', *, *, #8324, .T. ) ;
#5983 = CARTESIAN_POINT ( 'NONE',  ( 0.000000000000000000, -105.0000000000000711, 79.99999999999997158 ) ) ;
#5984 = ORIENTED_EDGE ( 'NONE', *, *, #6794, .T. ) ;
#5985 = CARTESIAN_POINT ( 'NONE',  ( 75.00000000000001421, 9.184850993605150311E-15, 0.000000000000000000 ) ) ;
#5986 = LINE ( 'NONE', #2775, #7550 ) ;
#5987 = CARTESIAN_POINT ( 'NONE',  ( 75.00000000000001421, 9.184850993605150311E-15, 20.00000000000000000 ) ) ;
#5988 = FACE_OUTER_BOUND ( 'NONE', #5525, .T. ) ;
#5989 = CARTESIAN_POINT ( 'NONE',  ( -105.0000000000000000, 72.50000000000000000, -212.5000000000000568 ) ) ;
#5990 = FACE_BOUND ( 'NONE', #6198, .T. ) ;
#5991 = FACE_OUTER_BOUND ( 'NONE', #6851, .T. ) ;
#5992 = ORIENTED_EDGE ( 'NONE', *, *, #462, .T. ) ;
#5993 = FACE_OUTER_BOUND ( 'NONE', #5069, .T. ) ;
#5994 = DIRECTION ( 'NONE',  ( 0.7071067811865474617, 8.659560562354932858E-17, 0.7071067811865474617 ) ) ;
#5995 = ORIENTED_EDGE ( 'NONE', *, *, #7896, .F. ) ;
#5996 = CARTESIAN_POINT ( 'NONE',  ( -75.00000000000001421, 0.000000000000000000, 57.99999999999999289 ) ) ;
#5997 = DIRECTION ( 'NONE',  ( 0.000000000000000000, 0.000000000000000000, 1.000000000000000000 ) ) ;
#5998 = CYLINDRICAL_SURFACE ( 'NONE', #2519, 14.99999999999998579 ) ;
#5999 = DIRECTION ( 'NONE',  ( -1.000000000000000000, -0.000000000000000000, -0.000000000000000000 ) ) ;
#6000 = CARTESIAN_POINT ( 'NONE',  ( 0.000000000000000000, -72.49999999999998579, 79.99999999999995737 ) ) ;
#6001 = ADVANCED_FACE ( 'NONE', ( #4553 ), #5000, .T. ) ;
#6002 = ORIENTED_EDGE ( 'NONE', *, *, #4776, .T. ) ;
#6003 = DIRECTION ( 'NONE',  ( -1.000000000000000000, -0.000000000000000000, -0.000000000000000000 ) ) ;
#6004 = DIRECTION ( 'NONE',  ( -0.000000000000000000, -0.000000000000000000, 1.000000000000000000 ) ) ;
#6005 = VERTEX_POINT ( 'NONE', #6261 ) ;
#6006 = MECHANICAL_DESIGN_GEOMETRIC_PRESENTATION_REPRESENTATION (  '', ( #2901 ), #6967 ) ;
#6007 = ORIENTED_EDGE ( 'NONE', *, *, #4204, .T. ) ;
#6008 = DIRECTION ( 'NONE',  ( 0.000000000000000000, 0.000000000000000000, 1.000000000000000000 ) ) ;
#6009 = CARTESIAN_POINT ( 'NONE',  ( -125.0000000000000000, -125.0000000000000284, 0.000000000000000000 ) ) ;
#6010 = CARTESIAN_POINT ( 'NONE',  ( -114.9999999999999858, -114.9999999999999858, 10.00000000000000000 ) ) ;
#6011 = EDGE_CURVE ( 'NONE', #3478, #4879, #691, .T. ) ;
#6012 = EDGE_CURVE ( 'NONE', #7934, #7988, #4305, .T. ) ;
#6013 = EDGE_CURVE ( 'NONE', #6134, #3849, #7688, .T. ) ;
#6014 = VECTOR ( 'NONE', #6812, 1000.000000000000000 ) ;
#6015 = EDGE_LOOP ( 'NONE', ( #601, #2555 ) ) ;
#6016 = ORIENTED_EDGE ( 'NONE', *, *, #1089, .T. ) ;
#6017 = CARTESIAN_POINT ( 'NONE',  ( -125.0000000000002558, -125.0000000000000000, 20.00000000000000000 ) ) ;
#6018 = EDGE_LOOP ( 'NONE', ( #7174, #7977, #6816, #7200 ) ) ;
#6019 = DIRECTION ( 'NONE',  ( 0.000000000000000000, 0.000000000000000000, 1.000000000000000000 ) ) ;
#6020 = AXIS2_PLACEMENT_3D ( 'NONE', #6252, #4814, #6116 ) ;
#6021 = CARTESIAN_POINT ( 'NONE',  ( 110.0000000000000142, 115.0000000000000000, 340.0000000000000000 ) ) ;
#6022 = VECTOR ( 'NONE', #2524, 1000.000000000000000 ) ;
#6023 = CARTESIAN_POINT ( 'NONE',  ( 120.0000000000000000, 115.0000000000000000, 270.0000000000000000 ) ) ;
#6024 = EDGE_CURVE ( 'NONE', #6622, #15, #5246, .T. ) ;
#6025 = CIRCLE ( 'NONE', #7810, 15.00000000000000000 ) ;
#6026 = DIRECTION ( 'NONE',  ( -0.000000000000000000, -1.000000000000000000, -0.000000000000000000 ) ) ;
#6027 = DIRECTION ( 'NONE',  ( -0.000000000000000000, -0.000000000000000000, 1.000000000000000000 ) ) ;
#6028 = CIRCLE ( 'NONE', #3741, 20.00000000000000355 ) ;
#6029 = FACE_BOUND ( 'NONE', #6333, .T. ) ;
#6030 = DIRECTION ( 'NONE',  ( 1.000000000000000000, 0.000000000000000000, 0.000000000000000000 ) ) ;
#6031 = PLANE ( 'NONE',  #2175 ) ;
#6032 = ORIENTED_EDGE ( 'NONE', *, *, #619, .F. ) ;
#6033 = VECTOR ( 'NONE', #6665, 1000.000000000000000 ) ;
#6034 = AXIS2_PLACEMENT_3D ( 'NONE', #1312, #8325, #3879 ) ;
#6035 = DIRECTION ( 'NONE',  ( -0.000000000000000000, -0.000000000000000000, 1.000000000000000000 ) ) ;
#6036 = EDGE_CURVE ( 'NONE', #6639, #7887, #1765, .T. ) ;
#6037 = ORIENTED_EDGE ( 'NONE', *, *, #2088, .T. ) ;
#6038 = AXIS2_PLACEMENT_3D ( 'NONE', #2170, #7139, #1364 ) ;
#6039 = ORIENTED_EDGE ( 'NONE', *, *, #6422, .F. ) ;
#6040 = DIRECTION ( 'NONE',  ( 0.000000000000000000, 0.5000000000000011102, 0.8660254037844380415 ) ) ;
#6041 = VECTOR ( 'NONE', #3305, 1000.000000000000114 ) ;
#6042 = AXIS2_PLACEMENT_3D ( 'NONE', #5892, #794, #4663 ) ;
#6043 = CARTESIAN_POINT ( 'NONE',  ( -99.99999999999990052, 115.0000000000000000, 250.0000000000000000 ) ) ;
#6044 = FACE_OUTER_BOUND ( 'NONE', #755, .T. ) ;
#6045 = DIRECTION ( 'NONE',  ( 1.000000000000000000, 0.000000000000000000, 0.000000000000000000 ) ) ;
#6046 = VECTOR ( 'NONE', #616, 1000.000000000000000 ) ;
#6047 = CIRCLE ( 'NONE', #5661, 4.999999999999990230 ) ;
#6048 = DIRECTION ( 'NONE',  ( 0.000000000000000000, 0.000000000000000000, -1.000000000000000000 ) ) ;
#6049 = ORIENTED_EDGE ( 'NONE', *, *, #6750, .T. ) ;
#6050 = CARTESIAN_POINT ( 'NONE',  ( 0.000000000000000000, -52.49999999999996447, 79.99999999999995737 ) ) ;
#6051 = DIRECTION ( 'NONE',  ( -1.000000000000000000, -0.000000000000000000, -0.000000000000000000 ) ) ;
#6052 = ORIENTED_EDGE ( 'NONE', *, *, #6250, .T. ) ;
#6053 = VECTOR ( 'NONE', #3121, 1000.000000000000000 ) ;
#6054 = ORIENTED_EDGE ( 'NONE', *, *, #2912, .T. ) ;
#6055 = DIRECTION ( 'NONE',  ( 1.000000000000000000, -0.000000000000000000, 0.000000000000000000 ) ) ;
#6056 = LINE ( 'NONE', #271, #185 ) ;
#6057 = FACE_OUTER_BOUND ( 'NONE', #6680, .T. ) ;
#6058 = ORIENTED_EDGE ( 'NONE', *, *, #7323, .F. ) ;
#6059 = PRODUCT_RELATED_PRODUCT_CATEGORY ( 'part', '', ( #1091 ) ) ;
#6060 = EDGE_LOOP ( 'NONE', ( #5414, #7899, #1959, #4325 ) ) ;
#6061 = CARTESIAN_POINT ( 'NONE',  ( -75.00000000000001421, 0.000000000000000000, 0.000000000000000000 ) ) ;
#6062 = VERTEX_POINT ( 'NONE', #484 ) ;
#6063 = ADVANCED_FACE ( 'NONE', ( #3008 ), #3051, .T. ) ;
#6064 = CARTESIAN_POINT ( 'NONE',  ( 0.000000000000000000, 0.000000000000000000, -248.3416876048222832 ) ) ;
#6065 = DIRECTION ( 'NONE',  ( 1.224646799147346798E-16, 3.155443620884047222E-30, -1.000000000000000000 ) ) ;
#6066 = ORIENTED_EDGE ( 'NONE', *, *, #7581, .F. ) ;
#6067 = CARTESIAN_POINT ( 'NONE',  ( 99.99999999999990052, 115.0000000000000000, 0.000000000000000000 ) ) ;
#6068 = CARTESIAN_POINT ( 'NONE',  ( 10.00000000000000000, -58.00000000000000711, 93.74999999999998579 ) ) ;
#6069 = EDGE_CURVE ( 'NONE', #6508, #1566, #7008, .T. ) ;
#6070 = DIRECTION ( 'NONE',  ( 0.000000000000000000, 0.000000000000000000, -1.000000000000000000 ) ) ;
#6071 = LINE ( 'NONE', #287, #3395 ) ;
#6072 = EDGE_CURVE ( 'NONE', #4767, #2601, #249, .T. ) ;
#6073 = CARTESIAN_POINT ( 'NONE',  ( -54.99999999999999289, -55.00000000000000711, 27.50000000000000000 ) ) ;
#6074 = EDGE_CURVE ( 'NONE', #3690, #5057, #6047, .T. ) ;
#6075 = ORIENTED_EDGE ( 'NONE', *, *, #1806, .F. ) ;
#6076 = VERTEX_POINT ( 'NONE', #4726 ) ;
#6077 = CARTESIAN_POINT ( 'NONE',  ( 5.000000000000000000, -2.342598717236898054, 4.057500000000003659 ) ) ;
#6078 = DIRECTION ( 'NONE',  ( 1.000000000000000000, 0.000000000000000000, 0.000000000000000000 ) ) ;
#6079 = CARTESIAN_POINT ( 'NONE',  ( -1.171242772578794285E-13, -12.50000000000001066, -12.49999999999997868 ) ) ;
#6080 = ORIENTED_EDGE ( 'NONE', *, *, #2322, .T. ) ;
#6081 = CARTESIAN_POINT ( 'NONE',  ( 0.000000000000000000, 72.49999999999994316, 240.0000000000000284 ) ) ;
#6082 = CARTESIAN_POINT ( 'NONE',  ( 54.99999999999999289, 55.00000000000000711, -27.50000000000000000 ) ) ;
#6083 = DIRECTION ( 'NONE',  ( -0.000000000000000000, -0.000000000000000000, 1.000000000000000000 ) ) ;
#6084 = ORIENTED_EDGE ( 'NONE', *, *, #8043, .F. ) ;
#6085 = CARTESIAN_POINT ( 'NONE',  ( 17.61817604250836311, -4.500000000000000000, -120.5000000000000284 ) ) ;
#6086 = DIRECTION ( 'NONE',  ( -1.460819769243625652E-16, 1.000000000000000000, 0.000000000000000000 ) ) ;
#6087 = ORIENTED_EDGE ( 'NONE', *, *, #1691, .F. ) ;
#6088 = CARTESIAN_POINT ( 'NONE',  ( 0.000000000000000000, 0.000000000000000000, -126.0000000000000284 ) ) ;
#6089 = EDGE_LOOP ( 'NONE', ( #275, #3262, #7135, #7505 ) ) ;
#6090 = CYLINDRICAL_SURFACE ( 'NONE', #6455, 15.00000000000000000 ) ;
#6091 = AXIS2_PLACEMENT_3D ( 'NONE', #526, #997, #1035 ) ;
#6092 = CARTESIAN_POINT ( 'NONE',  ( 10.00000000000000000, 54.99999999999989342, 93.75000000000004263 ) ) ;
#6093 = AXIS2_PLACEMENT_3D ( 'NONE', #5842, #325, #7841 ) ;
#6094 = CONTEXT_DEPENDENT_SHAPE_REPRESENTATION ( #7720, #7780 ) ;
#6095 = DIRECTION ( 'NONE',  ( 0.000000000000000000, 0.000000000000000000, 1.000000000000000000 ) ) ;
#6096 = CARTESIAN_POINT ( 'NONE',  ( 14.30908802125418511, 4.500000000000000000, -128.0000000000000284 ) ) ;
#6097 = ORIENTED_EDGE ( 'NONE', *, *, #6105, .T. ) ;
#6098 = CARTESIAN_POINT ( 'NONE',  ( 125.0000000000000000, -125.0000000000000000, 340.0000000000000000 ) ) ;
#6099 = ORIENTED_EDGE ( 'NONE', *, *, #8128, .T. ) ;
#6100 = FACE_OUTER_BOUND ( 'NONE', #3130, .T. ) ;
#6101 = DIRECTION ( 'NONE',  ( 1.224646799147346798E-16, 3.155443620884047222E-30, -1.000000000000000000 ) ) ;
#6102 = VERTEX_POINT ( 'NONE', #6595 ) ;
#6103 = CARTESIAN_POINT ( 'NONE',  ( 11.21327906667868390, 48.72680251680211683, -6.961169940684509783 ) ) ;
#6104 = DIRECTION ( 'NONE',  ( 0.000000000000000000, 0.000000000000000000, -1.000000000000000000 ) ) ;
#6105 = EDGE_CURVE ( 'NONE', #5480, #902, #2104, .T. ) ;
#6106 = CIRCLE ( 'NONE', #6792, 15.00000000000000000 ) ;
#6107 = DIRECTION ( 'NONE',  ( 1.000000000000000000, 0.000000000000000000, 0.000000000000000000 ) ) ;
#6108 = DIRECTION ( 'NONE',  ( 1.000000000000000000, 0.000000000000000000, 0.000000000000000000 ) ) ;
#6109 = DIRECTION ( 'NONE',  ( 0.000000000000000000, 0.000000000000000000, -1.000000000000000000 ) ) ;
#6110 = ORIENTED_EDGE ( 'NONE', *, *, #7581, .T. ) ;
#6111 = VERTEX_POINT ( 'NONE', #1529 ) ;
#6112 = APPLICATION_CONTEXT ( 'automotive_design' ) ;
#6113 = EDGE_CURVE ( 'NONE', #8056, #3183, #5450, .T. ) ;
#6114 = ADVANCED_FACE ( 'NONE', ( #3365 ), #4126, .F. ) ;
#6115 = ORIENTED_EDGE ( 'NONE', *, *, #5159, .F. ) ;
#6116 = DIRECTION ( 'NONE',  ( 1.000000000000000000, 0.000000000000000000, 0.000000000000000000 ) ) ;
#6117 = CARTESIAN_POINT ( 'NONE',  ( 114.9999999999999147, -115.0000000000000000, 0.000000000000000000 ) ) ;
#6118 = ORIENTED_EDGE ( 'NONE', *, *, #7448, .F. ) ;
#6119 = CARTESIAN_POINT ( 'NONE',  ( -10.82846484896509232, -48.81376096915063556, -6.242155733168281095 ) ) ;
#6120 =( NAMED_UNIT ( * ) PLANE_ANGLE_UNIT ( ) SI_UNIT ( $, .RADIAN. ) );
#6121 =( NAMED_UNIT ( * ) SI_UNIT ( $, .STERADIAN. ) SOLID_ANGLE_UNIT ( ) );
#6122 = DIRECTION ( 'NONE',  ( -0.000000000000000000, -0.000000000000000000, 1.000000000000000000 ) ) ;
#6123 = EDGE_CURVE ( 'NONE', #8125, #1093, #3491, .T. ) ;
#6124 = VERTEX_POINT ( 'NONE', #7871 ) ;
#6125 = FACE_BOUND ( 'NONE', #7445, .T. ) ;
#6126 = DIRECTION ( 'NONE',  ( 0.000000000000000000, 1.000000000000000000, -1.295896757998781966E-15 ) ) ;
#6127 = CARTESIAN_POINT ( 'NONE',  ( 95.00000000000000000, 95.00000000000008527, 35.00000000000000000 ) ) ;
#6128 = DIRECTION ( 'NONE',  ( 0.000000000000000000, -0.000000000000000000, -1.000000000000000000 ) ) ;
#6129 = AXIS2_PLACEMENT_3D ( 'NONE', #6160, #7527, #380 ) ;
#6130 = ORIENTED_EDGE ( 'NONE', *, *, #284, .F. ) ;
#6131 = DIRECTION ( 'NONE',  ( 1.000000000000000000, 0.000000000000000000, 0.000000000000000000 ) ) ;
#6132 = CARTESIAN_POINT ( 'NONE',  ( -114.9999999999999147, 99.99999999999998579, 250.0000000000000000 ) ) ;
#6133 = AXIS2_PLACEMENT_3D ( 'NONE', #23, #590, #7777 ) ;
#6134 = VERTEX_POINT ( 'NONE', #5327 ) ;
#6135 = FACE_OUTER_BOUND ( 'NONE', #4411, .T. ) ;
#6136 = VECTOR ( 'NONE', #6563, 1000.000000000000000 ) ;
#6137 = CARTESIAN_POINT ( 'NONE',  ( 79.17200000000011073, 0.000000000000000000, 0.000000000000000000 ) ) ;
#6138 = EDGE_CURVE ( 'NONE', #5179, #624, #6730, .T. ) ;
#6139 = AXIS2_PLACEMENT_3D ( 'NONE', #2108, #3369, #4649 ) ;
#6140 = PRODUCT_DEFINITION_CONTEXT ( 'detailed design', #523, 'design' ) ;
#6141 = EDGE_LOOP ( 'NONE', ( #2760, #7312, #7605, #3038 ) ) ;
#6142 = CARTESIAN_POINT ( 'NONE',  ( -99.99999999999991473, -115.0000000000000000, 250.0000000000000000 ) ) ;
#6143 = EDGE_LOOP ( 'NONE', ( #3719, #1722 ) ) ;
#6144 = FACE_BOUND ( 'NONE', #6599, .T. ) ;
#6145 = VERTEX_POINT ( 'NONE', #5290 ) ;
#6146 = ITEM_DEFINED_TRANSFORMATION ( 'NONE', 'NONE', #5433,  #1299 ) ;
#6147 = DIRECTION ( 'NONE',  ( -0.000000000000000000, -0.000000000000000000, 1.000000000000000000 ) ) ;
#6148 = CIRCLE ( 'NONE', #8329, 4.999999999999990230 ) ;
#6149 = VERTEX_POINT ( 'NONE', #7223 ) ;
#6150 = CARTESIAN_POINT ( 'NONE',  ( 125.0000000000000000, 52.50000000000000000, 190.0000000000000284 ) ) ;
#6151 = FACE_OUTER_BOUND ( 'NONE', #374, .T. ) ;
#6152 = VECTOR ( 'NONE', #4210, 1000.000000000000000 ) ;
#6153 = ORIENTED_EDGE ( 'NONE', *, *, #135, .T. ) ;
#6154 = DIRECTION ( 'NONE',  ( 1.000000000000000000, 0.000000000000000000, 0.000000000000000000 ) ) ;
#6155 = CIRCLE ( 'NONE', #7523, 54.99999999999995026 ) ;
#6156 = ORIENTED_EDGE ( 'NONE', *, *, #6011, .F. ) ;
#6157 = ORIENTED_EDGE ( 'NONE', *, *, #7602, .F. ) ;
#6158 = ORIENTED_EDGE ( 'NONE', *, *, #3930, .T. ) ;
#6159 = VECTOR ( 'NONE', #6673, 1000.000000000000000 ) ;
#6160 = CARTESIAN_POINT ( 'NONE',  ( 120.0000000000000000, 120.0000000000000000, -28.00000000000002487 ) ) ;
#6161 = ORIENTED_EDGE ( 'NONE', *, *, #7263, .F. ) ;
#6162 = AXIS2_PLACEMENT_3D ( 'NONE', #1740, #22, #7570 ) ;
#6163 = FACE_OUTER_BOUND ( 'NONE', #1738, .T. ) ;
#6164 = FACE_OUTER_BOUND ( 'NONE', #3149, .T. ) ;
#6165 = VECTOR ( 'NONE', #635, 1000.000000000000000 ) ;
#6166 = CYLINDRICAL_SURFACE ( 'NONE', #3772, 5.999999999999991118 ) ;
#6167 = ADVANCED_FACE ( 'NONE', ( #7271 ), #773, .F. ) ;
#6168 = EDGE_LOOP ( 'NONE', ( #2305, #3650, #711, #4559 ) ) ;
#6169 = CARTESIAN_POINT ( 'NONE',  ( -11.69960264931230220, -48.61219013327713157, -8.080179916824185682 ) ) ;
#6170 = ADVANCED_FACE ( 'NONE', ( #2223, #5364, #6631, #5990, #7945 ), #4806, .T. ) ;
#6171 = AXIS2_PLACEMENT_3D ( 'NONE', #5361, #4724, #817 ) ;
#6172 = ORIENTED_EDGE ( 'NONE', *, *, #3547, .F. ) ;
#6173 = ORIENTED_EDGE ( 'NONE', *, *, #2828, .F. ) ;
#6174 = VECTOR ( 'NONE', #3191, 1000.000000000000000 ) ;
#6175 = AXIS2_PLACEMENT_3D ( 'NONE', #2243, #398, #4218 ) ;
#6176 = CARTESIAN_POINT ( 'NONE',  ( 109.5000000000000142, -114.9999999999999716, 10.00000000000000000 ) ) ;
#6177 = CARTESIAN_POINT ( 'NONE',  ( 114.9999999999999147, -115.0000000000000000, 0.000000000000000000 ) ) ;
#6178 = DIRECTION ( 'NONE',  ( 1.000000000000000000, 0.000000000000000000, 0.000000000000000000 ) ) ;
#6179 = ORIENTED_EDGE ( 'NONE', *, *, #2925, .F. ) ;
#6180 = DIRECTION ( 'NONE',  ( 1.000000000000000000, 0.000000000000000000, 0.000000000000000000 ) ) ;
#6181 = EDGE_CURVE ( 'NONE', #7, #7108, #203, .T. ) ;
#6182 = EDGE_CURVE ( 'NONE', #2372, #2265, #7831, .T. ) ;
#6183 = FACE_OUTER_BOUND ( 'NONE', #7358, .T. ) ;
#6184 = CONICAL_SURFACE ( 'NONE', #2432, 4.999999999999990230, 1.029744258676653201 ) ;
#6185 = VECTOR ( 'NONE', #3640, 1000.000000000000114 ) ;
#6186 = FACE_OUTER_BOUND ( 'NONE', #7204, .T. ) ;
#6187 = ORIENTED_EDGE ( 'NONE', *, *, #6894, .F. ) ;
#6188 = AXIS2_PLACEMENT_3D ( 'NONE', #2113, #2642, #4571 ) ;
#6189 = COLOUR_RGB ( '',0.7921568627450980005, 0.8196078431372548767, 0.9333333333333333481 ) ;
#6190 = EDGE_LOOP ( 'NONE', ( #3788, #7191, #6535, #4409, #8171, #3493, #6910, #2639 ) ) ;
#6191 = DIRECTION ( 'NONE',  ( 1.000000000000000000, 0.000000000000000000, 0.000000000000000000 ) ) ;
#6192 = ORIENTED_EDGE ( 'NONE', *, *, #3549, .T. ) ;
#6193 = CARTESIAN_POINT ( 'NONE',  ( 0.000000000000000000, 0.000000000000000000, -6.999999999999999112 ) ) ;
#6194 = ADVANCED_FACE ( 'NONE', ( #7354 ), #1573, .T. ) ;
#6195 = FACE_OUTER_BOUND ( 'NONE', #1728, .T. ) ;
#6196 = APPLICATION_PROTOCOL_DEFINITION ( 'draft international standard', 'automotive_design', 1998, #8075 ) ;
#6197 = AXIS2_PLACEMENT_3D ( 'NONE', #1324, #3971, #3933 ) ;
#6198 = EDGE_LOOP ( 'NONE', ( #7301, #7890 ) ) ;
#6199 = PLANE ( 'NONE',  #5943 ) ;
#6200 = ADVANCED_FACE ( 'NONE', ( #1406 ), #3969, .F. ) ;
#6201 = CARTESIAN_POINT ( 'NONE',  ( -10.00000000000000000, -3.448762466456902719E-14, 93.74999999999998579 ) ) ;
#6202 = ORIENTED_EDGE ( 'NONE', *, *, #6181, .T. ) ;
#6203 = CARTESIAN_POINT ( 'NONE',  ( 10.00000000000000000, -3.448762466456902719E-14, 93.74999999999998579 ) ) ;
#6204 = EDGE_LOOP ( 'NONE', ( #775, #2507, #2710 ) ) ;
#6205 = DIRECTION ( 'NONE',  ( 0.000000000000000000, 0.000000000000000000, 1.000000000000000000 ) ) ;
#6206 = ORIENTED_EDGE ( 'NONE', *, *, #5562, .F. ) ;
#6207 = ORIENTED_EDGE ( 'NONE', *, *, #1273, .F. ) ;
#6208 = ORIENTED_EDGE ( 'NONE', *, *, #4024, .F. ) ;
#6209 = CIRCLE ( 'NONE', #6, 75.00000000000001421 ) ;
#6210 = CARTESIAN_POINT ( 'NONE',  ( -125.0000000000002558, -125.0000000000000000, 20.00000000000000000 ) ) ;
#6211 = CARTESIAN_POINT ( 'NONE',  ( -50.00000000000000711, 55.00000000000000000, 220.0000000000000284 ) ) ;
#6212 = VERTEX_POINT ( 'NONE', #373 ) ;
#6213 = SURFACE_STYLE_USAGE ( .BOTH. , #8078 ) ;
#6214 = AXIS2_PLACEMENT_3D ( 'NONE', #4713, #4150, #3427 ) ;
#6215 = VERTEX_POINT ( 'NONE', #7569 ) ;
#6216 = ORIENTED_EDGE ( 'NONE', *, *, #4720, .T. ) ;
#6217 = ADVANCED_FACE ( 'NONE', ( #4167 ), #3900, .T. ) ;
#6218 = ADVANCED_FACE ( 'NONE', ( #5491 ), #250, .T. ) ;
#6219 = CARTESIAN_POINT ( 'NONE',  ( 0.000000000000000000, 0.000000000000000000, -28.00000000000002487 ) ) ;
#6220 = CARTESIAN_POINT ( 'NONE',  ( -75.00000000000000000, 55.00000000000000711, 27.50000000000000000 ) ) ;
#6221 = EDGE_LOOP ( 'NONE', ( #2165, #5517 ) ) ;
#6222 = DIRECTION ( 'NONE',  ( 0.000000000000000000, 0.000000000000000000, -1.000000000000000000 ) ) ;
#6223 = DIRECTION ( 'NONE',  ( 0.000000000000000000, 0.000000000000000000, -1.000000000000000000 ) ) ;
#6224 = ORIENTED_EDGE ( 'NONE', *, *, #3122, .F. ) ;
#6225 = AXIS2_PLACEMENT_3D ( 'NONE', #5285, #7866, #6587 ) ;
#6226 = DIRECTION ( 'NONE',  ( -0.000000000000000000, -0.000000000000000000, 1.000000000000000000 ) ) ;
#6227 = EDGE_CURVE ( 'NONE', #6430, #1402, #331, .T. ) ;
#6228 = ADVANCED_FACE ( 'NONE', ( #4202 ), #2380, .F. ) ;
#6229 = AXIS2_PLACEMENT_3D ( 'NONE', #7924, #2195, #1589 ) ;
#6230 = ORIENTED_EDGE ( 'NONE', *, *, #470, .F. ) ;
#6231 = CARTESIAN_POINT ( 'NONE',  ( -50.00000000000000000, 55.00000000000000000, 240.0000000000000284 ) ) ;
#6232 = CARTESIAN_POINT ( 'NONE',  ( 0.000000000000000000, -4.500000000000000000, -126.0000000000000284 ) ) ;
#6233 = ORIENTED_EDGE ( 'NONE', *, *, #6423, .T. ) ;
#6234 = AXIS2_PLACEMENT_3D ( 'NONE', #6751, #5204, #2293 ) ;
#6235 = CYLINDRICAL_SURFACE ( 'NONE', #4272, 12.99999999999999822 ) ;
#6236 = DIRECTION ( 'NONE',  ( 0.000000000000000000, -1.000000000000000000, 0.000000000000000000 ) ) ;
#6237 = VERTEX_POINT ( 'NONE', #1110 ) ;
#6238 = CONTEXT_DEPENDENT_SHAPE_REPRESENTATION ( #2886, #7713 ) ;
#6239 = VERTEX_POINT ( 'NONE', #2900 ) ;
#6240 = CARTESIAN_POINT ( 'NONE',  ( 115.0000000000000000, 114.9999999999999716, 20.00000000000000000 ) ) ;
#6241 = ORIENTED_EDGE ( 'NONE', *, *, #4069, .F. ) ;
#6242 = CARTESIAN_POINT ( 'NONE',  ( -110.0000000000000142, 115.0000000000000000, 270.0000000000000000 ) ) ;
#6243 = VERTEX_POINT ( 'NONE', #1019 ) ;
#6244 = DIRECTION ( 'NONE',  ( 1.000000000000000000, 0.000000000000000000, 0.000000000000000000 ) ) ;
#6245 = DIRECTION ( 'NONE',  ( 1.000000000000000000, 0.000000000000000000, 0.000000000000000000 ) ) ;
#6246 = VERTEX_POINT ( 'NONE', #6286 ) ;
#6247 = ORIENTED_EDGE ( 'NONE', *, *, #3572, .T. ) ;
#6248 = ORIENTED_EDGE ( 'NONE', *, *, #2026, .F. ) ;
#6249 = VERTEX_POINT ( 'NONE', #3529 ) ;
#6250 = EDGE_CURVE ( 'NONE', #4486, #5147, #2692, .T. ) ;
#6251 = DIRECTION ( 'NONE',  ( -0.000000000000000000, -0.000000000000000000, 1.000000000000000000 ) ) ;
#6252 = CARTESIAN_POINT ( 'NONE',  ( -54.99999999999999289, 55.00000000000000711, 27.50000000000000000 ) ) ;
#6253 = DIRECTION ( 'NONE',  ( 0.000000000000000000, 0.000000000000000000, -1.000000000000000000 ) ) ;
#6254 = CONICAL_SURFACE ( 'NONE', #6530, 4.171999999999999709, 0.7853981633975609666 ) ;
#6255 = ORIENTED_EDGE ( 'NONE', *, *, #581, .F. ) ;
#6256 = CARTESIAN_POINT ( 'NONE',  ( -9.931622870156765259, -49.00592830463494209, -4.865363096503712903 ) ) ;
#6257 = ORIENTED_EDGE ( 'NONE', *, *, #1046, .T. ) ;
#6258 = ORIENTED_EDGE ( 'NONE', *, *, #2032, .T. ) ;
#6259 = COLOUR_RGB ( '',0.7921568627450980005, 0.8196078431372548767, 0.9333333333333333481 ) ;
#6260 = CARTESIAN_POINT ( 'NONE',  ( 49.00000000000000000, -55.00000000000000711, 27.50000000000000000 ) ) ;
#6261 = CARTESIAN_POINT ( 'NONE',  ( 0.000000000000000000, -2.342598717236898054, 4.057500000000003659 ) ) ;
#6262 = VERTEX_POINT ( 'NONE', #3033 ) ;
#6263 = CARTESIAN_POINT ( 'NONE',  ( -114.9999999999999716, 114.9999999999999858, 20.00000000000000000 ) ) ;
#6264 = CARTESIAN_POINT ( 'NONE',  ( 5.167842669270961586, -49.73365441721959002, -23.88900650468791298 ) ) ;
#6265 = ORIENTED_EDGE ( 'NONE', *, *, #1745, .F. ) ;
#6266 = FACE_BOUND ( 'NONE', #5728, .T. ) ;
#6267 = VERTEX_POINT ( 'NONE', #2300 ) ;
#6268 = LINE ( 'NONE', #2573, #5248 ) ;
#6269 = LINE ( 'NONE', #8233, #6972 ) ;
#6270 = VECTOR ( 'NONE', #2488, 1000.000000000000000 ) ;
#6271 = CARTESIAN_POINT ( 'NONE',  ( 105.0000000000000000, 105.0000000000000711, 340.0000000000000000 ) ) ;
#6272 = ORIENTED_EDGE ( 'NONE', *, *, #6975, .F. ) ;
#6273 = CARTESIAN_POINT ( 'NONE',  ( 0.000000000000000000, 2.342598717236902939, -4.057500000000001883 ) ) ;
#6274 = CARTESIAN_POINT ( 'NONE',  ( -125.0000000000000000, -125.0000000000000000, -28.00000000000002487 ) ) ;
#6275 = EDGE_CURVE ( 'NONE', #7952, #698, #6998, .T. ) ;
#6276 = VERTEX_POINT ( 'NONE', #3568 ) ;
#6277 = APPLICATION_PROTOCOL_DEFINITION ( 'draft international standard', 'automotive_design', 1998, #5427 ) ;
#6278 = EDGE_CURVE ( 'NONE', #8341, #1277, #4422, .T. ) ;
#6279 = DIRECTION ( 'NONE',  ( -1.000000000000000000, -0.000000000000000000, -0.000000000000000000 ) ) ;
#6280 = ORIENTED_EDGE ( 'NONE', *, *, #3279, .F. ) ;
#6281 = DIRECTION ( 'NONE',  ( 1.000000000000000000, 0.000000000000000000, 0.000000000000000000 ) ) ;
#6282 = AXIS2_PLACEMENT_3D ( 'NONE', #6509, #5203, #5294 ) ;
#6283 = DIRECTION ( 'NONE',  ( -0.000000000000000000, -0.000000000000000000, 1.000000000000000000 ) ) ;
#6284 = EDGE_LOOP ( 'NONE', ( #1422, #1020, #4666, #7192 ) ) ;
#6285 = APPLICATION_CONTEXT ( 'automotive_design' ) ;
#6286 = CARTESIAN_POINT ( 'NONE',  ( 114.9999999999999147, 99.99999999999998579, 0.000000000000000000 ) ) ;
#6287 = CARTESIAN_POINT ( 'NONE',  ( 108.9999999999999147, -115.0000000000000000, -28.00000000000002487 ) ) ;
#6288 = AXIS2_PLACEMENT_3D ( 'NONE', #6219, #2354, #347 ) ;
#6289 = ADVANCED_FACE ( 'NONE', ( #4895 ), #3082, .F. ) ;
#6290 = CARTESIAN_POINT ( 'NONE',  ( -10.84905357516155711, 48.81101040073316710, -6.237423197851057921 ) ) ;
#6291 = ORIENTED_EDGE ( 'NONE', *, *, #3333, .T. ) ;
#6292 = ORIENTED_EDGE ( 'NONE', *, *, #1803, .T. ) ;
#6293 = CIRCLE ( 'NONE', #4939, 5.999999999999991118 ) ;
#6294 = CARTESIAN_POINT ( 'NONE',  ( -125.0000000000000000, 125.0000000000000284, 0.000000000000000000 ) ) ;
#6295 = CARTESIAN_POINT ( 'NONE',  ( 0.000000000000000000, 125.0000000000000568, 79.99999999999992895 ) ) ;
#6296 = AXIS2_PLACEMENT_3D ( 'NONE', #3692, #8228, #2362 ) ;
#6297 = DIRECTION ( 'NONE',  ( 1.000000000000000000, 0.000000000000000000, 0.000000000000000000 ) ) ;
#6298 = ORIENTED_EDGE ( 'NONE', *, *, #1717, .T. ) ;
#6299 = EDGE_CURVE ( 'NONE', #3768, #5024, #255, .T. ) ;
#6300 = CARTESIAN_POINT ( 'NONE',  ( -120.0000000000000000, -115.0000000000000000, 340.0000000000000000 ) ) ;
#6301 = EDGE_CURVE ( 'NONE', #293, #4652, #4027, .T. ) ;
#6302 = CARTESIAN_POINT ( 'NONE',  ( 0.000000000000000000, 0.000000000000000000, 20.00000000000000355 ) ) ;
#6303 = VECTOR ( 'NONE', #1279, 1000.000000000000000 ) ;
#6304 = ORIENTED_EDGE ( 'NONE', *, *, #2915, .F. ) ;
#6305 = AXIS2_PLACEMENT_3D ( 'NONE', #7792, #2016, #122 ) ;
#6306 = VERTEX_POINT ( 'NONE', #5663 ) ;
#6307 = EDGE_CURVE ( 'NONE', #110, #6452, #5621, .T. ) ;
#6308 = DIRECTION ( 'NONE',  ( 1.000000000000000000, 0.000000000000000000, 0.000000000000000000 ) ) ;
#6309 = FACE_OUTER_BOUND ( 'NONE', #3570, .T. ) ;
#6310 = AXIS2_PLACEMENT_3D ( 'NONE', #3030, #4803, #1106 ) ;
#6311 = CARTESIAN_POINT ( 'NONE',  ( 0.000000000000000000, 0.000000000000000000, 0.000000000000000000 ) ) ;
#6312 = DIRECTION ( 'NONE',  ( 1.000000000000000000, 0.000000000000000000, 0.000000000000000000 ) ) ;
#6313 = CARTESIAN_POINT ( 'NONE',  ( 4.044723210857163131, -49.83770199522206212, -0.6652966195906406810 ) ) ;
#6314 = DIRECTION ( 'NONE',  ( 1.000000000000000000, 0.000000000000000000, 0.000000000000000000 ) ) ;
#6315 = SURFACE_STYLE_USAGE ( .BOTH. , #1811 ) ;
#6316 = AXIS2_PLACEMENT_3D ( 'NONE', #2292, #3517, #1011 ) ;
#6317 = AXIS2_PLACEMENT_3D ( 'NONE', #4880, #3476, #274 ) ;
#6318 = DIRECTION ( 'NONE',  ( 0.000000000000000000, -1.000000000000000000, 0.000000000000000000 ) ) ;
#6319 = ORIENTED_EDGE ( 'NONE', *, *, #2323, .T. ) ;
#6320 = UNCERTAINTY_MEASURE_WITH_UNIT (LENGTH_MEASURE( 1.000000000000000082E-05 ), #4638, 'distance_accuracy_value', 'NONE');
#6321 = VERTEX_POINT ( 'NONE', #8153 ) ;
#6322 = DIRECTION ( 'NONE',  ( 0.000000000000000000, 0.000000000000000000, 1.000000000000000000 ) ) ;
#6323 = CIRCLE ( 'NONE', #2036, 5.499999999999991118 ) ;
#6324 = AXIS2_PLACEMENT_3D ( 'NONE', #348, #2921, #6178 ) ;
#6325 = ORIENTED_EDGE ( 'NONE', *, *, #6903, .F. ) ;
#6326 = CARTESIAN_POINT ( 'NONE',  ( 10.00000000000000000, -58.00000000000000711, 93.74999999999998579 ) ) ;
#6327 = CARTESIAN_POINT ( 'NONE',  ( 105.0000000000000000, 72.49999999999997158, 19.99999999999998934 ) ) ;
#6328 = APPLICATION_PROTOCOL_DEFINITION ( 'draft international standard', 'automotive_design', 1998, #7154 ) ;
#6329 = VERTEX_POINT ( 'NONE', #8198 ) ;
#6330 = LINE ( 'NONE', #7823, #1927 ) ;
#6331 = CIRCLE ( 'NONE', #2691, 4.999999999999997335 ) ;
#6332 = AXIS2_PLACEMENT_3D ( 'NONE', #7521, #5540, #6109 ) ;
#6333 = EDGE_LOOP ( 'NONE', ( #1325, #4496 ) ) ;
#6334 = ADVANCED_FACE ( 'NONE', ( #2424 ), #1789, .F. ) ;
#6335 = CARTESIAN_POINT ( 'NONE',  ( 115.0000000000000000, 115.0000000000000000, 340.0000000000000000 ) ) ;
#6336 = ORIENTED_EDGE ( 'NONE', *, *, #721, .F. ) ;
#6337 = DIRECTION ( 'NONE',  ( -0.000000000000000000, -0.000000000000000000, 1.000000000000000000 ) ) ;
#6338 = VERTEX_POINT ( 'NONE', #8244 ) ;
#6339 = VERTEX_POINT ( 'NONE', #2466 ) ;
#6340 = EDGE_CURVE ( 'NONE', #2853, #5618, #7398, .T. ) ;
#6341 = EDGE_CURVE ( 'NONE', #4302, #6778, #1354, .T. ) ;
#6342 = CARTESIAN_POINT ( 'NONE',  ( -125.0000000000000000, -125.0000000000000000, -28.00000000000002487 ) ) ;
#6343 = ADVANCED_FACE ( 'NONE', ( #7136 ), #3762, .F. ) ;
#6344 = DIRECTION ( 'NONE',  ( 0.000000000000000000, -1.000000000000000000, 7.945337353457666666E-18 ) ) ;
#6345 = ORIENTED_EDGE ( 'NONE', *, *, #2186, .F. ) ;
#6346 = CARTESIAN_POINT ( 'NONE',  ( 6.123246359811209136E-15, -49.99999999999999289, -25.00000000000000000 ) ) ;
#6347 = DIRECTION ( 'NONE',  ( -0.9218685772373164111, 3.095340849193210523E-16, 0.3875026790906690444 ) ) ;
#6348 = ORIENTED_EDGE ( 'NONE', *, *, #980, .T. ) ;
#6349 = FACE_OUTER_BOUND ( 'NONE', #7715, .T. ) ;
#6350 = ADVANCED_FACE ( 'NONE', ( #2543 ), #7420, .F. ) ;
#6351 = AXIS2_PLACEMENT_3D ( 'NONE', #6695, #4187, #4876 ) ;
#6352 = CARTESIAN_POINT ( 'NONE',  ( 0.000000000000000000, 1.191800603018649864E-15, -100.0000000000000000 ) ) ;
#6353 = CARTESIAN_POINT ( 'NONE',  ( 11.83910760917652105, -48.57829327830486221, -16.53147691254503826 ) ) ;
#6354 = LINE ( 'NONE', #7072, #8316 ) ;
#6355 = CARTESIAN_POINT ( 'NONE',  ( -125.0000000000000000, -125.0000000000000568, -9.184850993605156622E-15 ) ) ;
#6356 = ORIENTED_EDGE ( 'NONE', *, *, #4633, .T. ) ;
#6357 = LINE ( 'NONE', #2526, #6635 ) ;
#6358 = VERTEX_POINT ( 'NONE', #1361 ) ;
#6359 = DIRECTION ( 'NONE',  ( 6.106226635438364917E-16, 3.154042683594196846E-17, 1.000000000000000000 ) ) ;
#6360 = EDGE_LOOP ( 'NONE', ( #1431, #6824 ) ) ;
#6361 = CARTESIAN_POINT ( 'NONE',  ( 125.0000000000000000, 125.0000000000000568, -9.184850993605156622E-15 ) ) ;
#6362 = DIRECTION ( 'NONE',  ( 0.000000000000000000, -0.000000000000000000, -1.000000000000000000 ) ) ;
#6363 = ORIENTED_EDGE ( 'NONE', *, *, #530, .F. ) ;
#6364 = CARTESIAN_POINT ( 'NONE',  ( 125.0000000000000000, 125.0000000000000568, 19.99999999999998934 ) ) ;
#6365 = ORIENTED_EDGE ( 'NONE', *, *, #6278, .F. ) ;
#6366 = CIRCLE ( 'NONE', #148, 5.999999999999991118 ) ;
#6367 = CARTESIAN_POINT ( 'NONE',  ( 125.0000000000000000, -125.0000000000000284, 70.00000000000000000 ) ) ;
#6368 = ORIENTED_EDGE ( 'NONE', *, *, #5224, .F. ) ;
#6369 = CARTESIAN_POINT ( 'NONE',  ( -10.00000000000000000, 54.99999999999989342, 93.75000000000004263 ) ) ;
#6370 = AXIS2_PLACEMENT_3D ( 'NONE', #278, #7877, #777 ) ;
#6371 = EDGE_CURVE ( 'NONE', #7416, #7579, #2625, .T. ) ;
#6372 = CARTESIAN_POINT ( 'NONE',  ( 5.000000000000000000, -2.342598717236898054, 4.057500000000003659 ) ) ;
#6373 = EDGE_CURVE ( 'NONE', #8146, #5670, #1875, .T. ) ;
#6374 = DIRECTION ( 'NONE',  ( 1.000000000000000000, 0.000000000000000000, 0.000000000000000000 ) ) ;
#6375 = FACE_OUTER_BOUND ( 'NONE', #1783, .T. ) ;
#6376 = CARTESIAN_POINT ( 'NONE',  ( 0.000000000000000000, 2.635170283421476540E-17, -246.6833752096445664 ) ) ;
#6377 = CARTESIAN_POINT ( 'NONE',  ( 0.000000000000000000, 0.000000000000000000, 0.000000000000000000 ) ) ;
#6378 = EDGE_CURVE ( 'NONE', #5057, #3690, #120, .T. ) ;
#6379 = CARTESIAN_POINT ( 'NONE',  ( 95.00000000000002842, -95.00000000000002842, 35.00000000000000000 ) ) ;
#6380 = EDGE_LOOP ( 'NONE', ( #5936, #909 ) ) ;
#6381 = CARTESIAN_POINT ( 'NONE',  ( -5.169052467613977520, -49.73353547763984039, -23.88849205255370123 ) ) ;
#6382 = EDGE_CURVE ( 'NONE', #402, #6651, #5702, .T. ) ;
#6383 = ADVANCED_FACE ( 'NONE', ( #5107 ), #7701, .F. ) ;
#6384 = ORIENTED_EDGE ( 'NONE', *, *, #1555, .T. ) ;
#6385 = DIRECTION ( 'NONE',  ( -1.000000000000000000, 0.000000000000000000, 0.000000000000000000 ) ) ;
#6386 = AXIS2_PLACEMENT_3D ( 'NONE', #6377, #7352, #5408 ) ;
#6387 = FACE_OUTER_BOUND ( 'NONE', #5572, .T. ) ;
#6388 = CARTESIAN_POINT ( 'NONE',  ( -102.5000000000000000, 0.000000000000000000, 0.000000000000000000 ) ) ;
#6389 = DIRECTION ( 'NONE',  ( 1.000000000000000000, 0.000000000000000000, 0.000000000000000000 ) ) ;
#6390 = DIRECTION ( 'NONE',  ( -1.000000000000000000, 0.000000000000000000, 0.000000000000000000 ) ) ;
#6391 = VECTOR ( 'NONE', #7298, 1000.000000000000000 ) ;
#6392 = VERTEX_POINT ( 'NONE', #555 ) ;
#6393 =( REPRESENTATION_RELATIONSHIP ('NONE','NONE', #6882, #1440 ) REPRESENTATION_RELATIONSHIP_WITH_TRANSFORMATION ( #5096 )SHAPE_REPRESENTATION_RELATIONSHIP( ) );
#6394 = UNCERTAINTY_MEASURE_WITH_UNIT (LENGTH_MEASURE( 1.000000000000000082E-05 ), #1508, 'distance_accuracy_value', 'NONE');
#6395 = ORIENTED_EDGE ( 'NONE', *, *, #1245, .T. ) ;
#6396 = CARTESIAN_POINT ( 'NONE',  ( 0.000000000000000000, -5.000000000000000000, 0.000000000000000000 ) ) ;
#6397 = ORIENTED_EDGE ( 'NONE', *, *, #1744, .F. ) ;
#6398 = LINE ( 'NONE', #6326, #104 ) ;
#6399 = CARTESIAN_POINT ( 'NONE',  ( 14.14213562373095279, 5.000000000000000000, 0.000000000000000000 ) ) ;
#6400 = ADVANCED_FACE ( 'NONE', ( #7014, #5020 ), #6406, .F. ) ;
#6401 = VERTEX_POINT ( 'NONE', #3161 ) ;
#6402 = CARTESIAN_POINT ( 'NONE',  ( 120.0000000000000000, -115.0000000000000000, 270.0000000000000000 ) ) ;
#6403 = CARTESIAN_POINT ( 'NONE',  ( -120.0000000000000000, -115.0000000000000000, 270.0000000000000000 ) ) ;
#6404 = CARTESIAN_POINT ( 'NONE',  ( -110.0000000000000142, -115.0000000000000000, 340.0000000000000000 ) ) ;
#6405 = ORIENTED_EDGE ( 'NONE', *, *, #8001, .T. ) ;
#6406 = PLANE ( 'NONE',  #1082 ) ;
#6407 = CARTESIAN_POINT ( 'NONE',  ( -10.16267929626374666, 48.95685099404312979, -19.78936650929338370 ) ) ;
#6408 = ORIENTED_EDGE ( 'NONE', *, *, #2088, .F. ) ;
#6409 = CARTESIAN_POINT ( 'NONE',  ( 54.99999999999999289, -54.99999999999999289, -27.50000000000000000 ) ) ;
#6410 = ORIENTED_EDGE ( 'NONE', *, *, #5671, .T. ) ;
#6411 = MANIFOLD_SOLID_BREP ( 'Revolve1', #4480 ) ;
#6412 = DIRECTION ( 'NONE',  ( -0.8571673007021116675, 1.049727191138617833E-16, 0.5150380749100552658 ) ) ;
#6413 = VECTOR ( 'NONE', #83, 1000.000000000000000 ) ;
#6414 = DIRECTION ( 'NONE',  ( -1.000000000000000000, 0.000000000000000000, 0.000000000000000000 ) ) ;
#6415 = ORIENTED_EDGE ( 'NONE', *, *, #1866, .F. ) ;
#6416 = SURFACE_STYLE_FILL_AREA ( #7622 ) ;
#6417 =( NAMED_UNIT ( * ) SI_UNIT ( $, .STERADIAN. ) SOLID_ANGLE_UNIT ( ) );
#6418 = ORIENTED_EDGE ( 'NONE', *, *, #462, .F. ) ;
#6419 = AXIS2_PLACEMENT_3D ( 'NONE', #1775, #4317, #1122 ) ;
#6420 = ORIENTED_EDGE ( 'NONE', *, *, #885, .T. ) ;
#6421 = DIRECTION ( 'NONE',  ( -0.000000000000000000, -0.000000000000000000, -1.000000000000000000 ) ) ;
#6422 = EDGE_CURVE ( 'NONE', #4485, #5610, #1833, .T. ) ;
#6423 = EDGE_CURVE ( 'NONE', #3808, #3986, #3882, .T. ) ;
#6424 = VECTOR ( 'NONE', #7575, 1000.000000000000000 ) ;
#6425 = CARTESIAN_POINT ( 'NONE',  ( -54.99999999999999289, -75.00000000000000000, -27.50000000000000000 ) ) ;
#6426 = CARTESIAN_POINT ( 'NONE',  ( 12.33692650994068174, -48.45417487488280983, -14.55343858072928676 ) ) ;
#6427 = CARTESIAN_POINT ( 'NONE',  ( 115.0000000000000000, 115.0000000000000000, 340.0000000000000000 ) ) ;
#6428 = AXIS2_PLACEMENT_3D ( 'NONE', #1463, #7119, #4524 ) ;
#6429 = DIRECTION ( 'NONE',  ( -0.000000000000000000, -0.000000000000000000, 1.000000000000000000 ) ) ;
#6430 = VERTEX_POINT ( 'NONE', #1196 ) ;
#6431 = VECTOR ( 'NONE', #4241, 1000.000000000000000 ) ;
#6432 = ORIENTED_EDGE ( 'NONE', *, *, #1134, .F. ) ;
#6433 = VECTOR ( 'NONE', #6885, 1000.000000000000000 ) ;
#6434 = EDGE_CURVE ( 'NONE', #5584, #5389, #5744, .T. ) ;
#6435 = ORIENTED_EDGE ( 'NONE', *, *, #6866, .F. ) ;
#6436 = CARTESIAN_POINT ( 'NONE',  ( -108.9999999999999147, -115.0000000000000000, -28.00000000000002487 ) ) ;
#6437 = ADVANCED_FACE ( 'NONE', ( #4758 ), #8230, .F. ) ;
#6438 = EDGE_LOOP ( 'NONE', ( #4476, #796, #723, #1689 ) ) ;
#6439 = LINE ( 'NONE', #3066, #4964 ) ;
#6440 = CARTESIAN_POINT ( 'NONE',  ( 95.00000000000002842, -95.00000000000002842, 35.00000000000000000 ) ) ;
#6441 = CARTESIAN_POINT ( 'NONE',  ( 125.0000000000000000, 125.0000000000000284, 70.00000000000000000 ) ) ;
#6442 = VECTOR ( 'NONE', #7173, 1000.000000000000000 ) ;
#6443 = CONTEXT_DEPENDENT_SHAPE_REPRESENTATION ( #1184, #2513 ) ;
#6444 = AXIS2_PLACEMENT_3D ( 'NONE', #985, #8069, #3573 ) ;
#6445 = CARTESIAN_POINT ( 'NONE',  ( 14.30908802125418511, -4.500000000000000000, -118.0000000000000284 ) ) ;
#6446 = ORIENTED_EDGE ( 'NONE', *, *, #5404, .F. ) ;
#6447 = AXIS2_PLACEMENT_3D ( 'NONE', #5817, #20, #7775 ) ;
#6448 = CIRCLE ( 'NONE', #2037, 50.00000000000000000 ) ;
#6449 = CARTESIAN_POINT ( 'NONE',  ( -109.5000000000000000, -114.9999999999999858, 0.000000000000000000 ) ) ;
#6450 = EDGE_CURVE ( 'NONE', #554, #3972, #3906, .T. ) ;
#6451 = LINE ( 'NONE', #8241, #790 ) ;
#6452 = VERTEX_POINT ( 'NONE', #4116 ) ;
#6453 = FILL_AREA_STYLE ('',( #638 ) ) ;
#6454 = ORIENTED_EDGE ( 'NONE', *, *, #419, .T. ) ;
#6455 = AXIS2_PLACEMENT_3D ( 'NONE', #315, #3596, #6180 ) ;
#6456 = VECTOR ( 'NONE', #437, 1000.000000000000000 ) ;
#6457 = CARTESIAN_POINT ( 'NONE',  ( -12.39753912377990019, 48.43864980223352745, -14.14916085730399331 ) ) ;
#6458 = EDGE_LOOP ( 'NONE', ( #3417, #1153, #1978, #5984 ) ) ;
#6459 = FACE_OUTER_BOUND ( 'NONE', #5466, .T. ) ;
#6460 = DIRECTION ( 'NONE',  ( -1.000000000000000000, 0.000000000000000000, 0.000000000000000000 ) ) ;
#6461 = AXIS2_PLACEMENT_3D ( 'NONE', #5299, #7882, #3297 ) ;
#6462 = AXIS2_PLACEMENT_3D ( 'NONE', #238, #2736, #1397 ) ;
#6463 = DIRECTION ( 'NONE',  ( 1.000000000000000000, 0.000000000000000000, 0.000000000000000000 ) ) ;
#6464 = CARTESIAN_POINT ( 'NONE',  ( 120.0000000000000000, -120.0000000000000000, -28.00000000000002487 ) ) ;
#6465 = DIRECTION ( 'NONE',  ( 1.000000000000000000, 0.000000000000000000, 0.000000000000000000 ) ) ;
#6466 = DIRECTION ( 'NONE',  ( -1.224646799147353207E-16, 1.000000000000000000, 1.874743562255115698E-31 ) ) ;
#6467 = CIRCLE ( 'NONE', #2824, 20.00000000000000355 ) ;
#6468 = ORIENTED_EDGE ( 'NONE', *, *, #3585, .F. ) ;
#6469 = ORIENTED_EDGE ( 'NONE', *, *, #4773, .T. ) ;
#6470 = DIRECTION ( 'NONE',  ( -0.000000000000000000, -0.000000000000000000, 1.000000000000000000 ) ) ;
#6471 = DIRECTION ( 'NONE',  ( -0.000000000000000000, -0.000000000000000000, 1.000000000000000000 ) ) ;
#6472 = DIRECTION ( 'NONE',  ( -0.000000000000000000, -7.945337353457666666E-18, -1.000000000000000000 ) ) ;
#6473 = CARTESIAN_POINT ( 'NONE',  ( 109.0000000000000142, 115.0000000000000000, 70.00000000000000000 ) ) ;
#6474 = PRODUCT_DEFINITION_SHAPE ( 'NONE', 'NONE',  #8355 ) ;
#6475 = DIRECTION ( 'NONE',  ( 1.000000000000000000, 0.000000000000000000, 0.000000000000000000 ) ) ;
#6476 = EDGE_CURVE ( 'NONE', #5497, #3934, #4574, .T. ) ;
#6477 = VERTEX_POINT ( 'NONE', #5902 ) ;
#6478 = DIRECTION ( 'NONE',  ( -0.000000000000000000, -0.000000000000000000, 1.000000000000000000 ) ) ;
#6479 = ORIENTED_EDGE ( 'NONE', *, *, #2430, .T. ) ;
#6480 = VERTEX_POINT ( 'NONE', #5985 ) ;
#6481 = DIRECTION ( 'NONE',  ( 1.000000000000000000, 0.000000000000000000, 0.000000000000000000 ) ) ;
#6482 = ORIENTED_EDGE ( 'NONE', *, *, #4296, .T. ) ;
#6483 = FACE_OUTER_BOUND ( 'NONE', #683, .T. ) ;
#6484 = CYLINDRICAL_SURFACE ( 'NONE', #2796, 54.99999999999996447 ) ;
#6485 = CONTEXT_DEPENDENT_SHAPE_REPRESENTATION ( #472, #6474 ) ;
#6486 = AXIS2_PLACEMENT_3D ( 'NONE', #5942, #5231, #3308 ) ;
#6487 = DIRECTION ( 'NONE',  ( -1.752490724247359037E-17, 1.000000000000000000, 3.853078496550133260E-17 ) ) ;
#6488 = EDGE_CURVE ( 'NONE', #1268, #3678, #2702, .T. ) ;
#6489 = EDGE_CURVE ( 'NONE', #2612, #7934, #194, .T. ) ;
#6490 = EDGE_CURVE ( 'NONE', #1935, #5539, #5237, .T. ) ;
#6491 = DIRECTION ( 'NONE',  ( 0.000000000000000000, 0.000000000000000000, -1.000000000000000000 ) ) ;
#6492 = ORIENTED_EDGE ( 'NONE', *, *, #3045, .T. ) ;
#6493 = CARTESIAN_POINT ( 'NONE',  ( 20.76917701662883076, 0.000000000000000000, 57.99999999999999289 ) ) ;
#6494 = VERTEX_POINT ( 'NONE', #761 ) ;
#6495 = DIRECTION ( 'NONE',  ( 0.000000000000000000, 1.000000000000000000, -1.632680918566406547E-16 ) ) ;
#6496 = ORIENTED_EDGE ( 'NONE', *, *, #3122, .T. ) ;
#6497 = DIRECTION ( 'NONE',  ( 0.000000000000000000, 0.000000000000000000, -1.000000000000000000 ) ) ;
#6498 = AXIS2_PLACEMENT_3D ( 'NONE', #3461, #4706, #1423 ) ;
#6499 = ORIENTED_EDGE ( 'NONE', *, *, #4296, .F. ) ;
#6500 = DIRECTION ( 'NONE',  ( 0.000000000000000000, 1.000000000000000000, 0.000000000000000000 ) ) ;
#6501 = ORIENTED_EDGE ( 'NONE', *, *, #7540, .F. ) ;
#6502 = MANIFOLD_SOLID_BREP ( 'Cut-Extrude4', #2230 ) ;
#6503 = LINE ( 'NONE', #4601, #8008 ) ;
#6504 = PLANE ( 'NONE',  #3749 ) ;
#6505 = DIRECTION ( 'NONE',  ( -1.000000000000000000, -0.000000000000000000, -0.000000000000000000 ) ) ;
#6506 = AXIS2_PLACEMENT_3D ( 'NONE', #2676, #3518, #2021 ) ;
#6507 = CARTESIAN_POINT ( 'NONE',  ( 9.999999999999998224, 0.000000000000000000, 0.000000000000000000 ) ) ;
#6508 = VERTEX_POINT ( 'NONE', #5947 ) ;
#6509 = CARTESIAN_POINT ( 'NONE',  ( 0.000000000000000000, 0.000000000000000000, 20.00000000000000000 ) ) ;
#6510 = DIRECTION ( 'NONE',  ( 1.224646799147348523E-16, 3.160065852750576588E-30, -1.000000000000000000 ) ) ;
#6511 = APPLICATION_CONTEXT ( 'automotive_design' ) ;
#6512 = DIRECTION ( 'NONE',  ( 0.000000000000000000, 0.000000000000000000, -1.000000000000000000 ) ) ;
#6513 = ADVANCED_FACE ( 'NONE', ( #2816 ), #2212, .F. ) ;
#6514 = EDGE_LOOP ( 'NONE', ( #5025, #7507, #2515, #7454, #4487 ) ) ;
#6515 = FACE_BOUND ( 'NONE', #3912, .T. ) ;
#6516 = CARTESIAN_POINT ( 'NONE',  ( 14.14213562373095279, 5.000000000000000000, 57.99999999999999289 ) ) ;
#6517 = AXIS2_PLACEMENT_3D ( 'NONE', #2177, #7308, #852 ) ;
#6518 = DIRECTION ( 'NONE',  ( 0.000000000000000000, 0.000000000000000000, -1.000000000000000000 ) ) ;
#6519 =( LENGTH_UNIT ( ) NAMED_UNIT ( * ) SI_UNIT ( .MILLI., .METRE. ) );
#6520 = CARTESIAN_POINT ( 'NONE',  ( 10.00000000000000000, -58.00000000000000711, 93.74999999999998579 ) ) ;
#6521 = ADVANCED_BREP_SHAPE_REPRESENTATION ( '', ( #3583, #1299 ), #7094 ) ;
#6522 = LINE ( 'NONE', #7849, #7384 ) ;
#6523 = ORIENTED_EDGE ( 'NONE', *, *, #2815, .T. ) ;
#6524 = DIRECTION ( 'NONE',  ( 0.000000000000000000, 0.000000000000000000, 1.000000000000000000 ) ) ;
#6525 = VERTEX_POINT ( 'NONE', #1479 ) ;
#6526 = CARTESIAN_POINT ( 'NONE',  ( 125.0000000000000000, -125.0000000000000568, -9.184850993605156622E-15 ) ) ;
#6527 = ORIENTED_EDGE ( 'NONE', *, *, #1990, .T. ) ;
#6528 = LINE ( 'NONE', #751, #8066 ) ;
#6529 = CARTESIAN_POINT ( 'NONE',  ( 105.0000000000000000, -72.49999999999994316, -212.5000000000000568 ) ) ;
#6530 = AXIS2_PLACEMENT_3D ( 'NONE', #2847, #7380, #6776 ) ;
#6531 = ITEM_DEFINED_TRANSFORMATION ( 'NONE', 'NONE', #5964,  #1299 ) ;
#6532 = DIRECTION ( 'NONE',  ( 0.000000000000000000, 0.000000000000000000, 1.000000000000000000 ) ) ;
#6533 = ORIENTED_EDGE ( 'NONE', *, *, #7797, .F. ) ;
#6534 = EDGE_CURVE ( 'NONE', #6339, #3044, #2699, .T. ) ;
#6535 = ORIENTED_EDGE ( 'NONE', *, *, #5274, .F. ) ;
#6536 = CARTESIAN_POINT ( 'NONE',  ( -95.00000000000001421, 0.000000000000000000, 15.00000000000000000 ) ) ;
#6537 = ORIENTED_EDGE ( 'NONE', *, *, #7806, .F. ) ;
#6538 = ADVANCED_FACE ( 'NONE', ( #846 ), #3620, .F. ) ;
#6539 = CARTESIAN_POINT ( 'NONE',  ( 99.49999999999998579, 0.000000000000000000, 0.000000000000000000 ) ) ;
#6540 = EDGE_CURVE ( 'NONE', #5497, #8000, #1523, .T. ) ;
#6541 = DIRECTION ( 'NONE',  ( 0.000000000000000000, 0.000000000000000000, -1.000000000000000000 ) ) ;
#6542 = CARTESIAN_POINT ( 'NONE',  ( 125.0000000000000000, -125.0000000000000284, 0.000000000000000000 ) ) ;
#6543 = EDGE_LOOP ( 'NONE', ( #8032, #2445, #515, #1510 ) ) ;
#6544 = FACE_BOUND ( 'NONE', #734, .T. ) ;
#6545 = CARTESIAN_POINT ( 'NONE',  ( 109.0000000000000426, -115.0000000000000000, 20.00000000000000355 ) ) ;
#6546 = LINE ( 'NONE', #771, #5238 ) ;
#6547 = EDGE_CURVE ( 'NONE', #6215, #6401, #7976, .T. ) ;
#6548 = CARTESIAN_POINT ( 'NONE',  ( 54.99999999999999289, 55.00000000000000711, 27.50000000000000000 ) ) ;
#6549 = PRODUCT_DEFINITION_SHAPE ( 'NONE', 'NONE',  #1585 ) ;
#6550 =( GEOMETRIC_REPRESENTATION_CONTEXT ( 3 ) GLOBAL_UNCERTAINTY_ASSIGNED_CONTEXT ( ( #3185 ) ) GLOBAL_UNIT_ASSIGNED_CONTEXT ( ( #1380, #3632, #4863 ) ) REPRESENTATION_CONTEXT ( 'NONE', 'WORKASPACE' ) );
#6551 = LINE ( 'NONE', #5957, #4435 ) ;
#6552 = ORIENTED_EDGE ( 'NONE', *, *, #4983, .F. ) ;
#6553 = DIRECTION ( 'NONE',  ( 2.643388153869419325E-16, -1.000000000000000000, -0.000000000000000000 ) ) ;
#6554 = DIRECTION ( 'NONE',  ( 1.000000000000000000, 0.000000000000000000, 0.000000000000000000 ) ) ;
#6555 = ORIENTED_EDGE ( 'NONE', *, *, #7578, .F. ) ;
#6556 = AXIS2_PLACEMENT_3D ( 'NONE', #6409, #75, #5156 ) ;
#6557 = PRESENTATION_LAYER_ASSIGNMENT (  '', '', ( #3862 ) ) ;
#6558 = CARTESIAN_POINT ( 'NONE',  ( 0.000000000000000000, 0.000000000000000000, 0.000000000000000000 ) ) ;
#6559 = AXIS2_PLACEMENT_3D ( 'NONE', #6740, #1131, #1673 ) ;
#6560 = EDGE_CURVE ( 'NONE', #2803, #4021, #5524, .T. ) ;
#6561 = APPLICATION_CONTEXT ( 'automotive_design' ) ;
#6562 = CYLINDRICAL_SURFACE ( 'NONE', #6461, 54.99999999999995026 ) ;
#6563 = DIRECTION ( 'NONE',  ( 1.000000000000000000, -0.000000000000000000, -0.000000000000000000 ) ) ;
#6564 = CIRCLE ( 'NONE', #4388, 57.99999999999995737 ) ;
#6565 = ADVANCED_FACE ( 'NONE', ( #8052 ), #1681, .F. ) ;
#6566 = PLANE ( 'NONE',  #646 ) ;
#6567 = EDGE_LOOP ( 'NONE', ( #7546, #6384, #5487, #8254 ) ) ;
#6568 = FACE_OUTER_BOUND ( 'NONE', #5329, .T. ) ;
#6569 = AXIS2_PLACEMENT_3D ( 'NONE', #5962, #2185, #861 ) ;
#6570 = CARTESIAN_POINT ( 'NONE',  ( -104.9999999999999432, -105.0000000000000853, 340.0000000000000000 ) ) ;
#6571 = AXIS2_PLACEMENT_3D ( 'NONE', #7922, #3542, #4704 ) ;
#6572 = ORIENTED_EDGE ( 'NONE', *, *, #6902, .T. ) ;
#6573 = DIRECTION ( 'NONE',  ( 0.000000000000000000, -0.000000000000000000, -1.000000000000000000 ) ) ;
#6574 = DIRECTION ( 'NONE',  ( 1.000000000000000000, 0.000000000000000000, 0.000000000000000000 ) ) ;
#6575 = AXIS2_PLACEMENT_3D ( 'NONE', #3240, #7048, #5146 ) ;
#6576 = DIRECTION ( 'NONE',  ( -1.000000000000000000, -0.000000000000000000, -0.000000000000000000 ) ) ;
#6577 = CIRCLE ( 'NONE', #4003, 5.000000000000035527 ) ;
#6578 = CYLINDRICAL_SURFACE ( 'NONE', #7258, 5.499999999999991118 ) ;
#6579 = VECTOR ( 'NONE', #6969, 1000.000000000000000 ) ;
#6580 = VERTEX_POINT ( 'NONE', #8015 ) ;
#6581 = CARTESIAN_POINT ( 'NONE',  ( -115.0000000000000000, 115.0000000000000000, 70.00000000000000000 ) ) ;
#6582 = AXIS2_PLACEMENT_3D ( 'NONE', #2737, #2664, #35 ) ;
#6583 = ORIENTED_EDGE ( 'NONE', *, *, #3482, .F. ) ;
#6584 = DIRECTION ( 'NONE',  ( -0.000000000000000000, -0.000000000000000000, -1.000000000000000000 ) ) ;
#6585 = VECTOR ( 'NONE', #2617, 1000.000000000000000 ) ;
#6586 = CIRCLE ( 'NONE', #2686, 12.50000000000000000 ) ;
#6587 = DIRECTION ( 'NONE',  ( 0.000000000000000000, 1.000000000000000000, 0.000000000000000000 ) ) ;
#6588 = EDGE_CURVE ( 'NONE', #7585, #3267, #243, .T. ) ;
#6589 = ORIENTED_EDGE ( 'NONE', *, *, #5713, .T. ) ;
#6590 = EDGE_CURVE ( 'NONE', #7108, #5161, #8101, .T. ) ;
#6591 = CARTESIAN_POINT ( 'NONE',  ( -114.9999999999999858, -114.9999999999999858, 20.00000000000000000 ) ) ;
#6592 = LINE ( 'NONE', #2739, #6159 ) ;
#6593 = DIRECTION ( 'NONE',  ( -0.000000000000000000, -1.000000000000000000, -0.000000000000000000 ) ) ;
#6594 = PLANE ( 'NONE',  #3680 ) ;
#6595 = CARTESIAN_POINT ( 'NONE',  ( 109.0000000000000142, 115.0000000000000000, 20.00000000000000355 ) ) ;
#6596 = AXIS2_PLACEMENT_3D ( 'NONE', #4390, #3105, #1216 ) ;
#6597 = AXIS2_PLACEMENT_3D ( 'NONE', #5637, #6505, #7791 ) ;
#6598 = DIRECTION ( 'NONE',  ( -0.000000000000000000, -0.000000000000000000, 1.000000000000000000 ) ) ;
#6599 = EDGE_LOOP ( 'NONE', ( #2339, #3775 ) ) ;
#6600 = FACE_BOUND ( 'NONE', #2309, .T. ) ;
#6601 = EDGE_CURVE ( 'NONE', #4386, #4206, #4697, .T. ) ;
#6602 = ADVANCED_FACE ( 'NONE', ( #6100 ), #6235, .F. ) ;
#6603 = EDGE_CURVE ( 'NONE', #7828, #2612, #6874, .T. ) ;
#6604 = AXIS2_PLACEMENT_3D ( 'NONE', #6064, #2256, #3020 ) ;
#6605 = DIRECTION ( 'NONE',  ( 1.000000000000000000, 0.000000000000000000, 0.000000000000000000 ) ) ;
#6606 = PRODUCT ( 'Lid', 'Lid', '', ( #1187 ) ) ;
#6607 = CYLINDRICAL_SURFACE ( 'NONE', #1550, 25.00000000000000000 ) ;
#6608 = DIRECTION ( 'NONE',  ( 1.000000000000000000, 0.000000000000000000, 0.000000000000000000 ) ) ;
#6609 = LINE ( 'NONE', #867, #6136 ) ;
#6610 = CIRCLE ( 'NONE', #6197, 12.99999999999999822 ) ;
#6611 = DIRECTION ( 'NONE',  ( 1.000000000000000000, 0.000000000000000000, 0.000000000000000000 ) ) ;
#6612 = DIRECTION ( 'NONE',  ( 1.000000000000000000, 0.000000000000000000, 0.000000000000000000 ) ) ;
#6613 = VERTEX_POINT ( 'NONE', #4193 ) ;
#6614 = DIRECTION ( 'NONE',  ( 1.000000000000000000, 0.000000000000000000, 0.000000000000000000 ) ) ;
#6615 = CARTESIAN_POINT ( 'NONE',  ( 0.000000000000000000, -5.000000000000000000, 0.000000000000000000 ) ) ;
#6616 = VERTEX_POINT ( 'NONE', #4159 ) ;
#6617 = ORIENTED_EDGE ( 'NONE', *, *, #1335, .F. ) ;
#6618 = DIRECTION ( 'NONE',  ( -1.000000000000000000, 0.000000000000000000, 0.000000000000000000 ) ) ;
#6619 = DIRECTION ( 'NONE',  ( -0.000000000000000000, -0.000000000000000000, 1.000000000000000000 ) ) ;
#6620 = DIRECTION ( 'NONE',  ( -0.000000000000000000, -0.000000000000000000, -1.000000000000000000 ) ) ;
#6621 = CIRCLE ( 'NONE', #968, 75.00000000000001421 ) ;
#6622 = VERTEX_POINT ( 'NONE', #3702 ) ;
#6623 = CYLINDRICAL_SURFACE ( 'NONE', #8212, 4.999999999999990230 ) ;
#6624 = ORIENTED_EDGE ( 'NONE', *, *, #5736, .T. ) ;
#6625 = DIRECTION ( 'NONE',  ( -1.000000000000000000, 0.000000000000000000, 0.000000000000000000 ) ) ;
#6626 = ADVANCED_BREP_SHAPE_REPRESENTATION ( '', ( #706, #1299 ), #7463 ) ;
#6627 = DIRECTION ( 'NONE',  ( 1.000000000000000000, 0.000000000000000000, 0.000000000000000000 ) ) ;
#6628 = LINE ( 'NONE', #3397, #7202 ) ;
#6629 = CARTESIAN_POINT ( 'NONE',  ( 55.00000000000000711, 54.99999999999999289, 27.50000000000000000 ) ) ;
#6630 = DIRECTION ( 'NONE',  ( -0.000000000000000000, 0.000000000000000000, -1.000000000000000000 ) ) ;
#6631 = FACE_BOUND ( 'NONE', #956, .T. ) ;
#6632 = CARTESIAN_POINT ( 'NONE',  ( 115.0000000000000000, -114.9999999999999716, 20.00000000000000000 ) ) ;
#6633 = DIRECTION ( 'NONE',  ( -0.000000000000000000, -0.000000000000000000, 1.000000000000000000 ) ) ;
#6634 = ADVANCED_FACE ( 'NONE', ( #4320, #6144 ), #5530, .F. ) ;
#6635 = VECTOR ( 'NONE', #582, 1000.000000000000000 ) ;
#6636 = ORIENTED_EDGE ( 'NONE', *, *, #1197, .F. ) ;
#6637 = CARTESIAN_POINT ( 'NONE',  ( 60.99999999999997868, 55.00000000000000711, -27.50000000000000000 ) ) ;
#6638 = CARTESIAN_POINT ( 'NONE',  ( 0.000000000000000000, 8.572527594031472204E-16, 6.999999999999999112 ) ) ;
#6639 = VERTEX_POINT ( 'NONE', #453 ) ;
#6640 = VERTEX_POINT ( 'NONE', #6193 ) ;
#6641 = FACE_OUTER_BOUND ( 'NONE', #3180, .T. ) ;
#6642 = ADVANCED_FACE ( 'NONE', ( #410 ), #324, .F. ) ;
#6643 = AXIS2_PLACEMENT_3D ( 'NONE', #2477, #8337, #5032 ) ;
#6644 = DIRECTION ( 'NONE',  ( 0.000000000000000000, 0.000000000000000000, -1.000000000000000000 ) ) ;
#6645 = DIRECTION ( 'NONE',  ( -0.000000000000000000, -0.000000000000000000, 1.000000000000000000 ) ) ;
#6646 = EDGE_CURVE ( 'NONE', #6243, #5161, #5608, .T. ) ;
#6647 = EDGE_CURVE ( 'NONE', #8288, #1049, #4794, .T. ) ;
#6648 = EDGE_CURVE ( 'NONE', #7972, #1294, #1065, .T. ) ;
#6649 = CARTESIAN_POINT ( 'NONE',  ( -109.5000000000000000, -114.9999999999999858, 10.00000000000000000 ) ) ;
#6650 = FACE_OUTER_BOUND ( 'NONE', #2361, .T. ) ;
#6651 = VERTEX_POINT ( 'NONE', #7472 ) ;
#6652 = CARTESIAN_POINT ( 'NONE',  ( 0.000000000000000000, -2.761866872635923494E-33, -100.0000000000000000 ) ) ;
#6653 = CLOSED_SHELL ( 'NONE', ( #6966, #188, #4619, #2578, #19, #4734, #4353, #1237, #2715, #1157, #1437, #7162, #7752, #3025, #4310, #4833, #496 ) ) ;
#6654 = DIRECTION ( 'NONE',  ( -1.000000000000000000, 0.000000000000000000, 0.000000000000000000 ) ) ;
#6655 = ORIENTED_EDGE ( 'NONE', *, *, #7807, .F. ) ;
#6656 = ORIENTED_EDGE ( 'NONE', *, *, #2649, .F. ) ;
#6657 = LINE ( 'NONE', #224, #8217 ) ;
#6658 = LINE ( 'NONE', #225, #2416 ) ;
#6659 = DIRECTION ( 'NONE',  ( 1.000000000000000000, 0.000000000000000000, 0.000000000000000000 ) ) ;
#6660 = VECTOR ( 'NONE', #7981, 1000.000000000000000 ) ;
#6661 = ORIENTED_EDGE ( 'NONE', *, *, #4642, .F. ) ;
#6662 = ORIENTED_EDGE ( 'NONE', *, *, #5314, .F. ) ;
#6663 = DIRECTION ( 'NONE',  ( -1.000000000000000000, 0.000000000000000000, 0.000000000000000000 ) ) ;
#6664 = ORIENTED_EDGE ( 'NONE', *, *, #5013, .T. ) ;
#6665 = DIRECTION ( 'NONE',  ( -1.000000000000000000, -0.000000000000000000, -0.000000000000000000 ) ) ;
#6666 = VECTOR ( 'NONE', #2187, 1000.000000000000000 ) ;
#6667 = ADVANCED_FACE ( 'NONE', ( #2412 ), #7434, .T. ) ;
#6668 = CARTESIAN_POINT ( 'NONE',  ( 0.000000000000000000, 7.945337353457666419E-16, -150.0000000000000000 ) ) ;
#6669 = CARTESIAN_POINT ( 'NONE',  ( -125.0000000000000000, 125.0000000000000000, 20.00000000000000000 ) ) ;
#6670 = DIRECTION ( 'NONE',  ( -1.752490724247359037E-17, 1.000000000000000000, 3.853078496550133260E-17 ) ) ;
#6671 =( REPRESENTATION_RELATIONSHIP ('NONE','NONE', #6882, #4267 ) REPRESENTATION_RELATIONSHIP_WITH_TRANSFORMATION ( #1304 )SHAPE_REPRESENTATION_RELATIONSHIP( ) );
#6672 = CARTESIAN_POINT ( 'NONE',  ( 125.0000000000000000, -125.0000000000000568, -9.184850993605156622E-15 ) ) ;
#6673 = DIRECTION ( 'NONE',  ( -1.000000000000000000, -0.000000000000000000, -0.000000000000000000 ) ) ;
#6674 = CARTESIAN_POINT ( 'NONE',  ( 95.00000000000000000, 95.00000000000008527, 70.00000000000000000 ) ) ;
#6675 = FACE_OUTER_BOUND ( 'NONE', #3778, .T. ) ;
#6676 = FACE_BOUND ( 'NONE', #7992, .T. ) ;
#6677 = CARTESIAN_POINT ( 'NONE',  ( 54.99999999999999289, 55.00000000000000711, 27.50000000000000000 ) ) ;
#6678 = DIRECTION ( 'NONE',  ( 0.000000000000000000, 1.000000000000000000, 0.000000000000000000 ) ) ;
#6679 = EDGE_LOOP ( 'NONE', ( #1816, #5302, #4088, #841 ) ) ;
#6680 = EDGE_LOOP ( 'NONE', ( #7376, #7165, #193 ) ) ;
#6681 = DIRECTION ( 'NONE',  ( -0.000000000000000000, -0.000000000000000000, 1.000000000000000000 ) ) ;
#6682 = LINE ( 'NONE', #905, #253 ) ;
#6683 = CARTESIAN_POINT ( 'NONE',  ( -114.9999999999999147, -115.0000000000000000, 250.0000000000000000 ) ) ;
#6684 = SURFACE_SIDE_STYLE ('',( #7324 ) ) ;
#6685 = DIRECTION ( 'NONE',  ( -0.000000000000000000, 0.000000000000000000, 1.000000000000000000 ) ) ;
#6686 = ORIENTED_EDGE ( 'NONE', *, *, #8326, .T. ) ;
#6687 = CONICAL_SURFACE ( 'NONE', #7370, 5.999999999999991118, 1.029744258676652313 ) ;
#6688 = EDGE_CURVE ( 'NONE', #8152, #3595, #2854, .T. ) ;
#6689 = EDGE_CURVE ( 'NONE', #1199, #6338, #1887, .T. ) ;
#6690 = DIRECTION ( 'NONE',  ( 1.000000000000000000, 0.000000000000000000, 0.000000000000000000 ) ) ;
#6691 = PRESENTATION_LAYER_ASSIGNMENT (  '', '', ( #2901 ) ) ;
#6692 = ORIENTED_EDGE ( 'NONE', *, *, #1817, .T. ) ;
#6693 = CARTESIAN_POINT ( 'NONE',  ( 0.000000000000000000, 72.49999999999997158, 19.99999999999998934 ) ) ;
#6694 = DIRECTION ( 'NONE',  ( 1.000000000000000000, 0.000000000000000000, 0.000000000000000000 ) ) ;
#6695 = CARTESIAN_POINT ( 'NONE',  ( 0.000000000000000000, 0.000000000000000000, 20.00000000000000355 ) ) ;
#6696 = VECTOR ( 'NONE', #7802, 1000.000000000000000 ) ;
#6697 = ADVANCED_FACE ( 'NONE', ( #1777 ), #5440, .F. ) ;
#6698 = ORIENTED_EDGE ( 'NONE', *, *, #4795, .F. ) ;
#6699 = CIRCLE ( 'NONE', #3057, 8.999999999999994671 ) ;
#6700 = ORIENTED_EDGE ( 'NONE', *, *, #1915, .T. ) ;
#6701 = PLANE ( 'NONE',  #6317 ) ;
#6702 = VERTEX_POINT ( 'NONE', #2458 ) ;
#6703 = CARTESIAN_POINT ( 'NONE',  ( 14.30908802125418511, 4.500000000000000000, -118.0000000000000284 ) ) ;
#6704 = CIRCLE ( 'NONE', #1591, 4.999999999999990230 ) ;
#6705 = CIRCLE ( 'NONE', #6571, 4.999999999999997335 ) ;
#6706 = ORIENTED_EDGE ( 'NONE', *, *, #6307, .F. ) ;
#6707 = CARTESIAN_POINT ( 'NONE',  ( 5.554896158147704988, 49.69628058154707162, -1.272184882194884903 ) ) ;
#6708 = EDGE_CURVE ( 'NONE', #1008, #7975, #3114, .T. ) ;
#6709 = EDGE_CURVE ( 'NONE', #7, #6243, #1998, .T. ) ;
#6710 = CIRCLE ( 'NONE', #6310, 4.057500000000000107 ) ;
#6711 = CYLINDRICAL_SURFACE ( 'NONE', #7121, 49.99999999999999289 ) ;
#6712 = AXIS2_PLACEMENT_3D ( 'NONE', #3352, #3425, #6694 ) ;
#6713 = PLANE ( 'NONE',  #7329 ) ;
#6714 = CARTESIAN_POINT ( 'NONE',  ( -114.9999999999999147, 0.000000000000000000, 250.0000000000000000 ) ) ;
#6715 = ORIENTED_EDGE ( 'NONE', *, *, #8193, .F. ) ;
#6716 = CARTESIAN_POINT ( 'NONE',  ( 121.0000000000000000, 115.0000000000000000, 20.00000000000000355 ) ) ;
#6717 = VECTOR ( 'NONE', #4710, 1000.000000000000000 ) ;
#6718 = CIRCLE ( 'NONE', #1060, 12.50000000000000000 ) ;
#6719 = DIRECTION ( 'NONE',  ( -0.000000000000000000, -0.000000000000000000, 1.000000000000000000 ) ) ;
#6720 = APPLICATION_CONTEXT ( 'automotive_design' ) ;
#6721 = ORIENTED_EDGE ( 'NONE', *, *, #3415, .F. ) ;
#6722 = DIRECTION ( 'NONE',  ( -1.321694076934710155E-16, 1.000000000000000000, 0.000000000000000000 ) ) ;
#6723 = CIRCLE ( 'NONE', #7825, 95.00000000000001421 ) ;
#6724 = VECTOR ( 'NONE', #2280, 1000.000000000000000 ) ;
#6725 = DIRECTION ( 'NONE',  ( -0.000000000000000000, 0.000000000000000000, 1.000000000000000000 ) ) ;
#6726 = CARTESIAN_POINT ( 'NONE',  ( 17.61817604250836311, 4.500000000000000000, -128.0000120000000265 ) ) ;
#6727 = ORIENTED_EDGE ( 'NONE', *, *, #5965, .T. ) ;
#6728 = SURFACE_STYLE_USAGE ( .BOTH. , #6684 ) ;
#6729 = VECTOR ( 'NONE', #2483, 1000.000000000000000 ) ;
#6730 = CIRCLE ( 'NONE', #7274, 4.999999999999990230 ) ;
#6731 = CARTESIAN_POINT ( 'NONE',  ( -109.0000000000000142, 115.0000000000000000, 70.00000000000000000 ) ) ;
#6732 = VERTEX_POINT ( 'NONE', #4490 ) ;
#6733 = FACE_BOUND ( 'NONE', #1746, .T. ) ;
#6734 = DIRECTION ( 'NONE',  ( -0.000000000000000000, -0.000000000000000000, 1.000000000000000000 ) ) ;
#6735 = VECTOR ( 'NONE', #3812, 1000.000000000000000 ) ;
#6736 = EDGE_LOOP ( 'NONE', ( #3908, #2688, #1963, #2726 ) ) ;
#6737 = VECTOR ( 'NONE', #5190, 1000.000000000000000 ) ;
#6738 = ORIENTED_EDGE ( 'NONE', *, *, #3693, .T. ) ;
#6739 = DIRECTION ( 'NONE',  ( -0.000000000000000000, 1.000000000000000000, -0.000000000000000000 ) ) ;
#6740 = CARTESIAN_POINT ( 'NONE',  ( 0.000000000000000000, 0.000000000000000000, 57.99999999999999289 ) ) ;
#6741 = EDGE_CURVE ( 'NONE', #2457, #5775, #4554, .T. ) ;
#6742 = DIRECTION ( 'NONE',  ( -0.000000000000000000, -0.000000000000000000, 1.000000000000000000 ) ) ;
#6743 = ORIENTED_EDGE ( 'NONE', *, *, #2767, .F. ) ;
#6744 = FACE_OUTER_BOUND ( 'NONE', #2748, .T. ) ;
#6745 = UNCERTAINTY_MEASURE_WITH_UNIT (LENGTH_MEASURE( 1.000000000000000082E-05 ), #2929, 'distance_accuracy_value', 'NONE');
#6746 = ORIENTED_EDGE ( 'NONE', *, *, #6341, .F. ) ;
#6747 = CARTESIAN_POINT ( 'NONE',  ( 5.000000000000000000, -2.342598717236898054, 4.057500000000003659 ) ) ;
#6748 = ORIENTED_EDGE ( 'NONE', *, *, #4437, .F. ) ;
#6749 = DIRECTION ( 'NONE',  ( -1.000000000000000000, -0.000000000000000000, -0.000000000000000000 ) ) ;
#6750 = EDGE_CURVE ( 'NONE', #7385, #3986, #8278, .T. ) ;
#6751 = CARTESIAN_POINT ( 'NONE',  ( -114.9999999999999858, 114.9999999999998863, 108.4000000000000341 ) ) ;
#6752 = EDGE_CURVE ( 'NONE', #6111, #4856, #5694, .T. ) ;
#6753 = ORIENTED_EDGE ( 'NONE', *, *, #1938, .T. ) ;
#6754 = CARTESIAN_POINT ( 'NONE',  ( 9.931622870156768812, 49.00592830463494920, -4.865363096503712903 ) ) ;
#6755 = CARTESIAN_POINT ( 'NONE',  ( 106.0000000000000142, 114.9999999999999716, 20.00000000000000000 ) ) ;
#6756 = CARTESIAN_POINT ( 'NONE',  ( 79.17200000000011073, 0.000000000000000000, 5.000000000000070166 ) ) ;
#6757 = CARTESIAN_POINT ( 'NONE',  ( 54.99999999999999289, 55.00000000000000000, 216.9956969048622284 ) ) ;
#6758 = DIRECTION ( 'NONE',  ( -0.000000000000000000, -0.000000000000000000, 1.000000000000000000 ) ) ;
#6759 = ORIENTED_EDGE ( 'NONE', *, *, #7362, .F. ) ;
#6760 = ORIENTED_EDGE ( 'NONE', *, *, #31, .T. ) ;
#6761 = ORIENTED_EDGE ( 'NONE', *, *, #6450, .T. ) ;
#6762 = DIRECTION ( 'NONE',  ( 0.000000000000000000, -0.000000000000000000, 1.000000000000000000 ) ) ;
#6763 = DIRECTION ( 'NONE',  ( -0.000000000000000000, -0.000000000000000000, 1.000000000000000000 ) ) ;
#6764 = ORIENTED_EDGE ( 'NONE', *, *, #6917, .T. ) ;
#6765 = EDGE_CURVE ( 'NONE', #1962, #471, #7642, .T. ) ;
#6766 = DIRECTION ( 'NONE',  ( 1.000000000000000000, 0.000000000000000000, 0.000000000000000000 ) ) ;
#6767 = CARTESIAN_POINT ( 'NONE',  ( -114.9999999999999147, -115.0000000000000000, 8.205133554287239938E-16 ) ) ;
#6768 = CARTESIAN_POINT ( 'NONE',  ( 120.5000000000000000, 114.9999999999999716, 0.000000000000000000 ) ) ;
#6769 = VECTOR ( 'NONE', #8131, 1000.000000000000000 ) ;
#6770 = EDGE_LOOP ( 'NONE', ( #2864, #2006 ) ) ;
#6771 = CARTESIAN_POINT ( 'NONE',  ( -50.00000000000000000, -55.00000000000000000, 240.0000000000000284 ) ) ;
#6772 = VERTEX_POINT ( 'NONE', #2496 ) ;
#6773 = DIRECTION ( 'NONE',  ( -0.000000000000000000, -0.000000000000000000, 1.000000000000000000 ) ) ;
#6774 = CARTESIAN_POINT ( 'NONE',  ( 50.00000000000000000, 55.00000000000000000, 240.0000000000000284 ) ) ;
#6775 = VERTEX_POINT ( 'NONE', #4401 ) ;
#6776 = DIRECTION ( 'NONE',  ( 0.000000000000000000, 0.000000000000000000, 1.000000000000000000 ) ) ;
#6777 = DIRECTION ( 'NONE',  ( 0.000000000000000000, 0.000000000000000000, 1.000000000000000000 ) ) ;
#6778 = VERTEX_POINT ( 'NONE', #497 ) ;
#6779 = PRODUCT_DEFINITION_CONTEXT ( 'detailed design', #8075, 'design' ) ;
#6780 = ORIENTED_EDGE ( 'NONE', *, *, #7157, .F. ) ;
#6781 = CARTESIAN_POINT ( 'NONE',  ( 115.0000000000000000, 114.9999999999999716, 10.00000000000000000 ) ) ;
#6782 = ORIENTED_EDGE ( 'NONE', *, *, #4837, .T. ) ;
#6783 = CARTESIAN_POINT ( 'NONE',  ( 0.000000000000000000, -4.500000000000000000, -128.0000120000000265 ) ) ;
#6784 = CIRCLE ( 'NONE', #598, 5.999999999999984901 ) ;
#6785 = CARTESIAN_POINT ( 'NONE',  ( -54.99999999999999289, 55.00000000000000000, -56.59999999999999432 ) ) ;
#6786 = ORIENTED_EDGE ( 'NONE', *, *, #7590, .T. ) ;
#6787 = CARTESIAN_POINT ( 'NONE',  ( -125.0000000000000000, 125.0000000000000000, 0.000000000000000000 ) ) ;
#6788 = EDGE_CURVE ( 'NONE', #1281, #4967, #1821, .T. ) ;
#6789 = CARTESIAN_POINT ( 'NONE',  ( -114.9999999999999147, 0.000000000000000000, 0.000000000000000000 ) ) ;
#6790 = LINE ( 'NONE', #369, #3136 ) ;
#6791 = EDGE_CURVE ( 'NONE', #5584, #1787, #7001, .T. ) ;
#6792 = AXIS2_PLACEMENT_3D ( 'NONE', #6088, #8222, #1767 ) ;
#6793 = CARTESIAN_POINT ( 'NONE',  ( -99.99999999999991473, -115.0000000000000000, 0.000000000000000000 ) ) ;
#6794 = EDGE_CURVE ( 'NONE', #4868, #8098, #589, .T. ) ;
#6795 = DIRECTION ( 'NONE',  ( 0.000000000000000000, 1.000000000000000000, 0.000000000000000000 ) ) ;
#6796 = DIRECTION ( 'NONE',  ( -0.000000000000000000, -0.000000000000000000, 1.000000000000000000 ) ) ;
#6797 = ORIENTED_EDGE ( 'NONE', *, *, #8299, .F. ) ;
#6798 = FILL_AREA_STYLE_COLOUR ( '', #7100 ) ;
#6799 = ORIENTED_EDGE ( 'NONE', *, *, #1655, .T. ) ;
#6800 = CARTESIAN_POINT ( 'NONE',  ( -105.0000000000000000, -105.0000000000000568, 20.00000000000004619 ) ) ;
#6801 = AXIS2_PLACEMENT_3D ( 'NONE', #186, #3555, #7970 ) ;
#6802 = ORIENTED_EDGE ( 'NONE', *, *, #5149, .F. ) ;
#6803 = ORIENTED_EDGE ( 'NONE', *, *, #5821, .T. ) ;
#6804 = ADVANCED_FACE ( 'NONE', ( #5735 ), #5093, .F. ) ;
#6805 = DIRECTION ( 'NONE',  ( -0.000000000000000000, 1.000000000000000000, 2.960594732333750610E-16 ) ) ;
#6806 = EDGE_CURVE ( 'NONE', #3292, #4851, #6439, .T. ) ;
#6807 = PRODUCT ( 'Bearing', 'Bearing', '', ( #4921 ) ) ;
#6808 = FACE_OUTER_BOUND ( 'NONE', #764, .T. ) ;
#6809 = ORIENTED_EDGE ( 'NONE', *, *, #8282, .T. ) ;
#6810 = ORIENTED_EDGE ( 'NONE', *, *, #5716, .T. ) ;
#6811 = ADVANCED_FACE ( 'NONE', ( #1182 ), #519, .F. ) ;
#6812 = DIRECTION ( 'NONE',  ( -1.460819769243625652E-16, 1.000000000000000000, 0.000000000000000000 ) ) ;
#6813 = EDGE_CURVE ( 'NONE', #4314, #984, #5374, .T. ) ;
#6814 = LINE ( 'NONE', #4781, #1743 ) ;
#6815 = CIRCLE ( 'NONE', #209, 9.500000000000008882 ) ;
#6816 = ORIENTED_EDGE ( 'NONE', *, *, #5563, .F. ) ;
#6817 = LINE ( 'NONE', #8126, #2043 ) ;
#6818 = CARTESIAN_POINT ( 'NONE',  ( 95.00000000000001421, 1.163414459189985801E-14, 15.00000000000000000 ) ) ;
#6819 = VECTOR ( 'NONE', #5213, 1000.000000000000000 ) ;
#6820 = CARTESIAN_POINT ( 'NONE',  ( -54.99999999999999289, -75.00000000000000000, 27.50000000000000000 ) ) ;
#6821 = AXIS2_PLACEMENT_3D ( 'NONE', #2717, #1459, #214 ) ;
#6822 = DIRECTION ( 'NONE',  ( -0.000000000000000000, -0.000000000000000000, 1.000000000000000000 ) ) ;
#6823 = CONICAL_SURFACE ( 'NONE', #2774, 5.999999999999991118, 1.029744258676652313 ) ;
#6824 = ORIENTED_EDGE ( 'NONE', *, *, #6648, .T. ) ;
#6825 = DIRECTION ( 'NONE',  ( -1.000000000000000000, -0.000000000000000000, -0.000000000000000000 ) ) ;
#6826 = EDGE_LOOP ( 'NONE', ( #5174, #6692, #6099, #6499 ) ) ;
#6827 = CARTESIAN_POINT ( 'NONE',  ( -10.00000000000000000, -55.00000000000000711, 93.74999999999998579 ) ) ;
#6828 = CARTESIAN_POINT ( 'NONE',  ( 95.00000000000002842, -95.00000000000002842, 70.00000000000000000 ) ) ;
#6829 =( REPRESENTATION_RELATIONSHIP ('NONE','NONE', #6882, #239 ) REPRESENTATION_RELATIONSHIP_WITH_TRANSFORMATION ( #3509 )SHAPE_REPRESENTATION_RELATIONSHIP( ) );
#6830 = ORIENTED_EDGE ( 'NONE', *, *, #3428, .T. ) ;
#6831 = APPLICATION_PROTOCOL_DEFINITION ( 'draft international standard', 'automotive_design', 1998, #523 ) ;
#6832 = DIRECTION ( 'NONE',  ( -1.000000000000000000, -0.000000000000000000, -0.000000000000000000 ) ) ;
#6833 = ORIENTED_EDGE ( 'NONE', *, *, #5013, .F. ) ;
#6834 = FACE_OUTER_BOUND ( 'NONE', #1286, .T. ) ;
#6835 = CARTESIAN_POINT ( 'NONE',  ( -104.9999999999999432, -105.0000000000000853, 340.0000000000000000 ) ) ;
#6836 = ORIENTED_EDGE ( 'NONE', *, *, #688, .T. ) ;
#6837 = DIRECTION ( 'NONE',  ( 1.000000000000000000, 0.000000000000000000, 0.000000000000000000 ) ) ;
#6838 = PLANE ( 'NONE',  #1328 ) ;
#6839 = DIRECTION ( 'NONE',  ( -0.8571673007021134438, 1.049727191138620051E-16, 0.5150380749100522682 ) ) ;
#6840 = VECTOR ( 'NONE', #8209, 1000.000000000000000 ) ;
#6841 = VERTEX_POINT ( 'NONE', #3747 ) ;
#6842 = DIRECTION ( 'NONE',  ( -0.000000000000000000, -0.000000000000000000, 1.000000000000000000 ) ) ;
#6843 = EDGE_LOOP ( 'NONE', ( #687, #7641, #7574, #6066 ) ) ;
#6844 = SURFACE_STYLE_USAGE ( .BOTH. , #947 ) ;
#6845 = EDGE_CURVE ( 'NONE', #7120, #5018, #938, .T. ) ;
#6846 = ORIENTED_EDGE ( 'NONE', *, *, #2860, .T. ) ;
#6847 = VECTOR ( 'NONE', #7665, 1000.000000000000000 ) ;
#6848 = CARTESIAN_POINT ( 'NONE',  ( -125.0000000000000000, -125.0000000000000568, -9.184850993605156622E-15 ) ) ;
#6849 = AXIS2_PLACEMENT_3D ( 'NONE', #6781, #1009, #6191 ) ;
#6850 = DIRECTION ( 'NONE',  ( 1.000000000000000000, 0.000000000000000000, 0.000000000000000000 ) ) ;
#6851 = EDGE_LOOP ( 'NONE', ( #3356, #456, #143, #3885 ) ) ;
#6852 = CYLINDRICAL_SURFACE ( 'NONE', #5500, 54.99999999999995026 ) ;
#6853 = EDGE_CURVE ( 'NONE', #6276, #6237, #1350, .T. ) ;
#6854 = EDGE_CURVE ( 'NONE', #6338, #1199, #3604, .T. ) ;
#6855 = EDGE_CURVE ( 'NONE', #718, #5007, #6398, .T. ) ;
#6856 = EDGE_LOOP ( 'NONE', ( #5165, #8249 ) ) ;
#6857 = VECTOR ( 'NONE', #7508, 1000.000000000000000 ) ;
#6858 = VECTOR ( 'NONE', #1224, 1000.000000000000000 ) ;
#6859 = DIRECTION ( 'NONE',  ( 0.000000000000000000, 1.000000000000000000, -1.224646799147353207E-16 ) ) ;
#6860 = CARTESIAN_POINT ( 'NONE',  ( 0.000000000000000000, -2.075330319324761228E-16, -251.3416876048222832 ) ) ;
#6861 = LINE ( 'NONE', #2880, #7133 ) ;
#6862 = VERTEX_POINT ( 'NONE', #5052 ) ;
#6863 = CYLINDRICAL_SURFACE ( 'NONE', #5912, 95.00000000000008527 ) ;
#6864 = DIRECTION ( 'NONE',  ( -0.000000000000000000, -0.000000000000000000, 1.000000000000000000 ) ) ;
#6865 = AXIS2_PLACEMENT_3D ( 'NONE', #6908, #4700, #5997 ) ;
#6866 = EDGE_CURVE ( 'NONE', #5233, #2019, #2807, .T. ) ;
#6867 = CYLINDRICAL_SURFACE ( 'NONE', #5225, 5.999999999999991118 ) ;
#6868 = VERTEX_POINT ( 'NONE', #183 ) ;
#6869 = CIRCLE ( 'NONE', #1760, 57.99999999999995737 ) ;
#6870 = AXIS2_PLACEMENT_3D ( 'NONE', #5867, #4416, #1964 ) ;
#6871 = ORIENTED_EDGE ( 'NONE', *, *, #4577, .T. ) ;
#6872 = LINE ( 'NONE', #5527, #4548 ) ;
#6873 = ORIENTED_EDGE ( 'NONE', *, *, #2616, .T. ) ;
#6874 = LINE ( 'NONE', #8138, #6857 ) ;
#6875 = CARTESIAN_POINT ( 'NONE',  ( 0.000000000000000000, 5.000000000000000000, 0.000000000000000000 ) ) ;
#6876 = EDGE_LOOP ( 'NONE', ( #5946, #4292, #1741 ) ) ;
#6877 = APPLICATION_PROTOCOL_DEFINITION ( 'draft international standard', 'automotive_design', 1998, #6285 ) ;
#6878 = VECTOR ( 'NONE', #2635, 1000.000000000000000 ) ;
#6879 = ORIENTED_EDGE ( 'NONE', *, *, #7662, .F. ) ;
#6880 = CARTESIAN_POINT ( 'NONE',  ( -125.0000000000002558, -125.0000000000000000, 20.00000000000000000 ) ) ;
#6881 = DIRECTION ( 'NONE',  ( 0.000000000000000000, 0.000000000000000000, 1.000000000000000000 ) ) ;
#6882 = SHAPE_REPRESENTATION ( 'MAT-045', ( #298, #1125, #165, #5837, #6643, #5433, #7742, #2859, #990, #3137, #3945, #4068, #6506, #7873, #4884, #6234, #6093, #5569, #7600, #849, #26, #1660, #5964, #1944, #2609, #6370 ), #7318 ) ;
#6883 = ORIENTED_EDGE ( 'NONE', *, *, #5821, .F. ) ;
#6884 = CARTESIAN_POINT ( 'NONE',  ( 115.0000000000000000, -114.9999999999999716, 20.00000000000000000 ) ) ;
#6885 = DIRECTION ( 'NONE',  ( -0.000000000000000000, -0.000000000000000000, 1.000000000000000000 ) ) ;
#6886 = ORIENTED_EDGE ( 'NONE', *, *, #5100, .T. ) ;
#6887 = VERTEX_POINT ( 'NONE', #4667 ) ;
#6888 = EDGE_LOOP ( 'NONE', ( #5812, #4259 ) ) ;
#6889 = DIRECTION ( 'NONE',  ( 1.000000000000000000, 0.000000000000000000, 0.000000000000000000 ) ) ;
#6890 = ORIENTED_EDGE ( 'NONE', *, *, #2597, .T. ) ;
#6891 = AXIS2_PLACEMENT_3D ( 'NONE', #3437, #4163, #2334 ) ;
#6892 = CARTESIAN_POINT ( 'NONE',  ( 105.0000000000000000, -72.49999999999994316, 20.00000000000002842 ) ) ;
#6893 = CARTESIAN_POINT ( 'NONE',  ( 0.000000000000000000, -15.00000000000000000, -120.5000000000000284 ) ) ;
#6894 = EDGE_CURVE ( 'NONE', #1112, #5179, #5310, .T. ) ;
#6895 = DIRECTION ( 'NONE',  ( 0.000000000000000000, 1.000000000000000000, 0.000000000000000000 ) ) ;
#6896 = VERTEX_POINT ( 'NONE', #4065 ) ;
#6897 =( LENGTH_UNIT ( ) NAMED_UNIT ( * ) SI_UNIT ( .MILLI., .METRE. ) );
#6898 = CIRCLE ( 'NONE', #4731, 4.999999999999990230 ) ;
#6899 = SURFACE_SIDE_STYLE ('',( #1758 ) ) ;
#6900 = ORIENTED_EDGE ( 'NONE', *, *, #7263, .T. ) ;
#6901 = DIRECTION ( 'NONE',  ( 1.000000000000000000, 0.000000000000000000, 0.000000000000000000 ) ) ;
#6902 = EDGE_CURVE ( 'NONE', #7887, #3072, #5856, .T. ) ;
#6903 = EDGE_CURVE ( 'NONE', #1049, #3183, #7207, .T. ) ;
#6904 = LINE ( 'NONE', #2444, #3773 ) ;
#6905 = ADVANCED_FACE ( 'NONE', ( #7296 ), #1428, .F. ) ;
#6906 = CARTESIAN_POINT ( 'NONE',  ( 120.0000000000000000, -120.0000000000000000, -28.00000000000002487 ) ) ;
#6907 = ORIENTED_EDGE ( 'NONE', *, *, #2597, .F. ) ;
#6908 = CARTESIAN_POINT ( 'NONE',  ( -31.74999999999995737, 0.000000000000000000, 0.000000000000000000 ) ) ;
#6909 = DIRECTION ( 'NONE',  ( -0.000000000000000000, -0.000000000000000000, 1.000000000000000000 ) ) ;
#6910 = ORIENTED_EDGE ( 'NONE', *, *, #4651, .T. ) ;
#6911 = TOROIDAL_SURFACE ( 'NONE', #8268, 5.400000000000035882, 0.4000000000000000222 ) ;
#6912 = CARTESIAN_POINT ( 'NONE',  ( 14.14213562373095279, 5.000000000000000000, 0.000000000000000000 ) ) ;
#6913 = ORIENTED_EDGE ( 'NONE', *, *, #7179, .T. ) ;
#6914 = ADVANCED_FACE ( 'NONE', ( #1514, #5977 ), #2762, .F. ) ;
#6915 = CIRCLE ( 'NONE', #5022, 12.49999999999999289 ) ;
#6916 = ORIENTED_EDGE ( 'NONE', *, *, #5263, .T. ) ;
#6917 = EDGE_CURVE ( 'NONE', #2291, #6401, #2729, .T. ) ;
#6918 = CARTESIAN_POINT ( 'NONE',  ( 114.9999999999999147, 115.0000000000000000, 8.205133554287239938E-16 ) ) ;
#6919 = CARTESIAN_POINT ( 'NONE',  ( -115.0000000000000000, 115.0000000000000000, 270.0000000000000000 ) ) ;
#6920 = DIRECTION ( 'NONE',  ( 1.000000000000000000, 0.000000000000000000, 0.000000000000000000 ) ) ;
#6921 = ORIENTED_EDGE ( 'NONE', *, *, #2388, .F. ) ;
#6922 = DIRECTION ( 'NONE',  ( 1.000000000000000000, 0.000000000000000000, 0.000000000000000000 ) ) ;
#6923 = DIRECTION ( 'NONE',  ( 0.000000000000000000, 0.000000000000000000, 1.000000000000000000 ) ) ;
#6924 = ORIENTED_EDGE ( 'NONE', *, *, #7851, .T. ) ;
#6925 = PRODUCT_CONTEXT ( 'NONE', #5427, 'mechanical' ) ;
#6926 = DIRECTION ( 'NONE',  ( 1.000000000000000000, 0.000000000000000000, 0.000000000000000000 ) ) ;
#6927 = ORIENTED_EDGE ( 'NONE', *, *, #721, .T. ) ;
#6928 = VERTEX_POINT ( 'NONE', #7168 ) ;
#6929 = EDGE_CURVE ( 'NONE', #6868, #4386, #6528, .T. ) ;
#6930 = CARTESIAN_POINT ( 'NONE',  ( 7.342598717236928252, 0.000000000000000000, 0.000000000000000000 ) ) ;
#6931 = ORIENTED_EDGE ( 'NONE', *, *, #3133, .F. ) ;
#6932 = DIRECTION ( 'NONE',  ( 1.000000000000000000, 0.000000000000000000, 0.000000000000000000 ) ) ;
#6933 = CARTESIAN_POINT ( 'NONE',  ( 114.9999999999999147, 115.0000000000000000, -28.00000000000002487 ) ) ;
#6934 = DIRECTION ( 'NONE',  ( 0.000000000000000000, -0.000000000000000000, 1.000000000000000000 ) ) ;
#6935 = EDGE_LOOP ( 'NONE', ( #5103, #5004, #6037, #7446 ) ) ;
#6936 = AXIS2_PLACEMENT_3D ( 'NONE', #2727, #2200, #7247 ) ;
#6937 = EDGE_LOOP ( 'NONE', ( #1018, #2596, #3502, #7525 ) ) ;
#6938 = DIRECTION ( 'NONE',  ( 0.000000000000000000, 0.000000000000000000, 1.000000000000000000 ) ) ;
#6939 = CARTESIAN_POINT ( 'NONE',  ( 115.0000000000000000, 114.9999999999999716, 20.00000000000000000 ) ) ;
#6940 = DIRECTION ( 'NONE',  ( 1.000000000000000000, 0.000000000000000000, 0.000000000000000000 ) ) ;
#6941 = AXIS2_PLACEMENT_3D ( 'NONE', #1169, #531, #7153 ) ;
#6942 = ORIENTED_EDGE ( 'NONE', *, *, #1988, .F. ) ;
#6943 = ORIENTED_EDGE ( 'NONE', *, *, #3079, .T. ) ;
#6944 = DIRECTION ( 'NONE',  ( 1.000000000000000000, 0.000000000000000000, 0.000000000000000000 ) ) ;
#6945 =( REPRESENTATION_RELATIONSHIP ('NONE','NONE', #6882, #239 ) REPRESENTATION_RELATIONSHIP_WITH_TRANSFORMATION ( #5229 )SHAPE_REPRESENTATION_RELATIONSHIP( ) );
#6946 = CARTESIAN_POINT ( 'NONE',  ( -95.00000000000008527, 1.163414459189986590E-14, 20.00000000000000355 ) ) ;
#6947 = PLANE ( 'NONE',  #6941 ) ;
#6948 = CARTESIAN_POINT ( 'NONE',  ( 0.000000000000000000, 0.000000000000000000, -250.0000000000000000 ) ) ;
#6949 = PRODUCT_DEFINITION ( 'UNKNOWN', '', #8121, #5730 ) ;
#6950 = CARTESIAN_POINT ( 'NONE',  ( -60.00000000000000000, 55.00000000000000000, 240.0000000000000284 ) ) ;
#6951 = PRODUCT_DEFINITION_SHAPE ( 'NONE', 'NONE',  #8372 ) ;
#6952 = EDGE_CURVE ( 'NONE', #5584, #6430, #3891, .T. ) ;
#6953 = VERTEX_POINT ( 'NONE', #5344 ) ;
#6954 = ORIENTED_EDGE ( 'NONE', *, *, #3961, .T. ) ;
#6955 = CARTESIAN_POINT ( 'NONE',  ( 99.49999999999998579, 0.000000000000000000, 12.50000000000000000 ) ) ;
#6956 = DIRECTION ( 'NONE',  ( -0.000000000000000000, -0.000000000000000000, 1.000000000000000000 ) ) ;
#6957 = ORIENTED_EDGE ( 'NONE', *, *, #7065, .T. ) ;
#6958 = DIRECTION ( 'NONE',  ( -0.7071067811864679697, 0.000000000000000000, 0.7071067811866271757 ) ) ;
#6959 = CARTESIAN_POINT ( 'NONE',  ( 115.0000000000000000, -114.9999999999999716, 20.00000000000000000 ) ) ;
#6960 = ORIENTED_EDGE ( 'NONE', *, *, #4091, .F. ) ;
#6961 = SHAPE_DEFINITION_REPRESENTATION ( #5536, #1440 ) ;
#6962 = VECTOR ( 'NONE', #8290, 1000.000000000000000 ) ;
#6963 = EDGE_LOOP ( 'NONE', ( #4782, #6115, #4489, #960 ) ) ;
#6964 = CARTESIAN_POINT ( 'NONE',  ( 0.000000000000000000, 0.000000000000000000, 57.99999999999999289 ) ) ;
#6965 = EDGE_CURVE ( 'NONE', #6005, #4856, #7928, .T. ) ;
#6966 = ADVANCED_FACE ( 'NONE', ( #2694 ), #5227, .T. ) ;
#6967 =( GEOMETRIC_REPRESENTATION_CONTEXT ( 3 ) GLOBAL_UNCERTAINTY_ASSIGNED_CONTEXT ( ( #491 ) ) GLOBAL_UNIT_ASSIGNED_CONTEXT ( ( #6982, #8296, #7062 ) ) REPRESENTATION_CONTEXT ( 'NONE', 'WORKASPACE' ) );
#6968 = ORIENTED_EDGE ( 'NONE', *, *, #3430, .F. ) ;
#6969 = DIRECTION ( 'NONE',  ( -0.000000000000000000, -0.000000000000000000, 1.000000000000000000 ) ) ;
#6970 = ORIENTED_EDGE ( 'NONE', *, *, #295, .T. ) ;
#6971 = DIRECTION ( 'NONE',  ( -1.000000000000000000, -0.000000000000000000, -0.000000000000000000 ) ) ;
#6972 = VECTOR ( 'NONE', #7598, 1000.000000000000114 ) ;
#6973 = ORIENTED_EDGE ( 'NONE', *, *, #8157, .T. ) ;
#6974 = ORIENTED_EDGE ( 'NONE', *, *, #973, .F. ) ;
#6975 = EDGE_CURVE ( 'NONE', #5646, #2109, #7891, .T. ) ;
#6976 = ORIENTED_EDGE ( 'NONE', *, *, #830, .F. ) ;
#6977 = CIRCLE ( 'NONE', #3193, 4.057500000000000107 ) ;
#6978 = DIRECTION ( 'NONE',  ( 1.000000000000000000, 0.000000000000000000, 0.000000000000000000 ) ) ;
#6979 = AXIS2_PLACEMENT_3D ( 'NONE', #6000, #345, #4096 ) ;
#6980 = DIRECTION ( 'NONE',  ( 0.000000000000000000, 7.945337353457666666E-18, 1.000000000000000000 ) ) ;
#6981 = EDGE_LOOP ( 'NONE', ( #7146, #2167, #7772 ) ) ;
#6982 =( LENGTH_UNIT ( ) NAMED_UNIT ( * ) SI_UNIT ( .MILLI., .METRE. ) );
#6983 = DIRECTION ( 'NONE',  ( 0.02014134804572967688, -5.590347086839542934E-18, 0.9997971424738624213 ) ) ;
#6984 = ORIENTED_EDGE ( 'NONE', *, *, #5928, .T. ) ;
#6985 = DIRECTION ( 'NONE',  ( -1.000000000000000000, 0.000000000000000000, 0.000000000000000000 ) ) ;
#6986 = CONICAL_SURFACE ( 'NONE', #2801, 9.500000000000008882, 0.7853981633974466137 ) ;
#6987 = DIRECTION ( 'NONE',  ( -0.000000000000000000, -0.000000000000000000, 1.000000000000000000 ) ) ;
#6988 = FACE_OUTER_BOUND ( 'NONE', #6284, .T. ) ;
#6989 = CARTESIAN_POINT ( 'NONE',  ( 75.00000000000001421, 9.184850993605150311E-15, 35.00000000000000000 ) ) ;
#6990 = AXIS2_PLACEMENT_3D ( 'NONE', #1388, #6008, #878 ) ;
#6991 = AXIS2_PLACEMENT_3D ( 'NONE', #6615, #7293, #3913 ) ;
#6992 = CARTESIAN_POINT ( 'NONE',  ( 5.000000000000000000, -2.342598717236898054, 4.057500000000003659 ) ) ;
#6993 = ORIENTED_EDGE ( 'NONE', *, *, #1283, .F. ) ;
#6994 = ORIENTED_EDGE ( 'NONE', *, *, #2836, .F. ) ;
#6995 = UNCERTAINTY_MEASURE_WITH_UNIT (LENGTH_MEASURE( 1.000000000000000082E-05 ), #5461, 'distance_accuracy_value', 'NONE');
#6996 = ORIENTED_EDGE ( 'NONE', *, *, #1643, .F. ) ;
#6997 = LINE ( 'NONE', #5969, #108 ) ;
#6998 = CIRCLE ( 'NONE', #3342, 5.000000000000004441 ) ;
#6999 = ORIENTED_EDGE ( 'NONE', *, *, #7626, .F. ) ;
#7000 = EDGE_CURVE ( 'NONE', #8106, #5384, #6657, .T. ) ;
#7001 = LINE ( 'NONE', #3150, #2289 ) ;
#7002 = FACE_OUTER_BOUND ( 'NONE', #5153, .T. ) ;
#7003 = ORIENTED_EDGE ( 'NONE', *, *, #6301, .F. ) ;
#7004 = ORIENTED_EDGE ( 'NONE', *, *, #2345, .T. ) ;
#7005 = CARTESIAN_POINT ( 'NONE',  ( 10.82421258667008246, 48.81470695058815323, -18.76526308057256287 ) ) ;
#7006 = AXIS2_PLACEMENT_3D ( 'NONE', #1888, #6980, #6344 ) ;
#7007 = ORIENTED_EDGE ( 'NONE', *, *, #5378, .T. ) ;
#7008 = CIRCLE ( 'NONE', #7948, 5.499999999999991118 ) ;
#7009 = EDGE_CURVE ( 'NONE', #426, #929, #4748, .T. ) ;
#7010 = ORIENTED_EDGE ( 'NONE', *, *, #6709, .F. ) ;
#7011 = CARTESIAN_POINT ( 'NONE',  ( -10.00000000000000000, -58.00000000000000711, 93.74999999999998579 ) ) ;
#7012 = ORIENTED_EDGE ( 'NONE', *, *, #6648, .F. ) ;
#7013 = ADVANCED_FACE ( 'NONE', ( #7856 ), #6184, .F. ) ;
#7014 = FACE_BOUND ( 'NONE', #2492, .T. ) ;
#7015 = ADVANCED_FACE ( 'NONE', ( #6483 ), #4029, .T. ) ;
#7016 = AXIS2_PLACEMENT_3D ( 'NONE', #6507, #3209, #5160 ) ;
#7017 = CARTESIAN_POINT ( 'NONE',  ( -12.50025679328619077, 48.41222552385477229, -11.67941733774922142 ) ) ;
#7018 = DIRECTION ( 'NONE',  ( -1.000000000000000000, 0.000000000000000000, 0.000000000000000000 ) ) ;
#7019 = ORIENTED_EDGE ( 'NONE', *, *, #4381, .T. ) ;
#7020 = DIRECTION ( 'NONE',  ( 1.000000000000000000, 0.000000000000000000, 0.000000000000000000 ) ) ;
#7021 = CARTESIAN_POINT ( 'NONE',  ( 0.000000000000000000, 105.0000000000000426, 79.99999999999992895 ) ) ;
#7022 = DIRECTION ( 'NONE',  ( 6.106226635438361958E-16, 0.000000000000000000, 1.000000000000000000 ) ) ;
#7023 = ADVANCED_FACE ( 'NONE', ( #4627 ), #3507, .F. ) ;
#7024 = CARTESIAN_POINT ( 'NONE',  ( 115.0000000000000000, -115.0000000000000000, 340.0000000000000000 ) ) ;
#7025 = EDGE_LOOP ( 'NONE', ( #4175, #3039, #3881, #4889 ) ) ;
#7026 = DIRECTION ( 'NONE',  ( -0.000000000000000000, -0.000000000000000000, 1.000000000000000000 ) ) ;
#7027 = AXIS2_PLACEMENT_3D ( 'NONE', #3026, #7046, #5659 ) ;
#7028 = DIRECTION ( 'NONE',  ( 1.000000000000000000, 0.000000000000000000, 0.000000000000000000 ) ) ;
#7029 = EDGE_CURVE ( 'NONE', #306, #3000, #3341, .T. ) ;
#7030 = VECTOR ( 'NONE', #8092, 1000.000000000000000 ) ;
#7031 = CARTESIAN_POINT ( 'NONE',  ( -114.9999999999999716, 114.9999999999999858, 10.00000000000000000 ) ) ;
#7032 = DIRECTION ( 'NONE',  ( -0.000000000000000000, 0.000000000000000000, 1.000000000000000000 ) ) ;
#7033 = CARTESIAN_POINT ( 'NONE',  ( 11.69966253144280799, -48.61218256317028619, -16.92010850872652128 ) ) ;
#7034 = CARTESIAN_POINT ( 'NONE',  ( -125.0000000000000000, 125.0000000000000284, 70.00000000000000000 ) ) ;
#7035 = LINE ( 'NONE', #6520, #5590 ) ;
#7036 = CYLINDRICAL_SURFACE ( 'NONE', #2407, 4.999999999999997335 ) ;
#7037 = ORIENTED_EDGE ( 'NONE', *, *, #7055, .F. ) ;
#7038 = ORIENTED_EDGE ( 'NONE', *, *, #1285, .F. ) ;
#7039 = ORIENTED_EDGE ( 'NONE', *, *, #4164, .T. ) ;
#7040 = CARTESIAN_POINT ( 'NONE',  ( 25.00000000000000000, 3.061616997868383043E-15, -120.5000000000000284 ) ) ;
#7041 = ORIENTED_EDGE ( 'NONE', *, *, #2835, .T. ) ;
#7042 = DIRECTION ( 'NONE',  ( 1.000000000000000000, 0.000000000000000000, 0.000000000000000000 ) ) ;
#7043 = CIRCLE ( 'NONE', #1795, 5.000000000000004441 ) ;
#7044 = CYLINDRICAL_SURFACE ( 'NONE', #4787, 75.00000000000001421 ) ;
#7045 = EDGE_LOOP ( 'NONE', ( #2384, #101, #1657, #2941 ) ) ;
#7046 = DIRECTION ( 'NONE',  ( 0.000000000000000000, 0.000000000000000000, -1.000000000000000000 ) ) ;
#7047 = PRODUCT_DEFINITION_FORMATION_WITH_SPECIFIED_SOURCE ( 'ANY', '', #1091, .NOT_KNOWN. ) ;
#7048 = DIRECTION ( 'NONE',  ( -0.000000000000000000, -0.000000000000000000, 1.000000000000000000 ) ) ;
#7049 = VERTEX_POINT ( 'NONE', #4784 ) ;
#7050 = DIRECTION ( 'NONE',  ( 0.000000000000000000, 1.000000000000000000, -0.000000000000000000 ) ) ;
#7051 = EDGE_CURVE ( 'NONE', #717, #4180, #2882, .T. ) ;
#7052 = CYLINDRICAL_SURFACE ( 'NONE', #4744, 57.99999999999995737 ) ;
#7053 = CARTESIAN_POINT ( 'NONE',  ( -9.400408038818907741, 49.10908733398244408, -20.74923976180172858 ) ) ;
#7054 = CARTESIAN_POINT ( 'NONE',  ( -25.00000000000000000, 0.000000000000000000, -126.0000000000000284 ) ) ;
#7055 = EDGE_CURVE ( 'NONE', #1566, #6508, #107, .T. ) ;
#7056 = EDGE_CURVE ( 'NONE', #6778, #7, #3473, .T. ) ;
#7057 = CARTESIAN_POINT ( 'NONE',  ( -114.9999999999999147, -115.0000000000000000, 8.205133554287239938E-16 ) ) ;
#7058 = AXIS2_PLACEMENT_3D ( 'NONE', #7983, #1528, #4645 ) ;
#7059 = DIRECTION ( 'NONE',  ( 0.000000000000000000, 1.000000000000000000, 0.000000000000000000 ) ) ;
#7060 = DIRECTION ( 'NONE',  ( 1.000000000000000000, 0.000000000000000000, 0.000000000000000000 ) ) ;
#7061 = FACE_OUTER_BOUND ( 'NONE', #3227, .T. ) ;
#7062 =( NAMED_UNIT ( * ) SI_UNIT ( $, .STERADIAN. ) SOLID_ANGLE_UNIT ( ) );
#7063 = ORIENTED_EDGE ( 'NONE', *, *, #2034, .F. ) ;
#7064 = DIRECTION ( 'NONE',  ( -0.000000000000000000, -0.000000000000000000, 1.000000000000000000 ) ) ;
#7065 = EDGE_CURVE ( 'NONE', #14, #4729, #6323, .T. ) ;
#7066 = ADVANCED_FACE ( 'NONE', ( #4222 ), #6090, .T. ) ;
#7067 = DIRECTION ( 'NONE',  ( -0.7071067811864679697, 8.659560562355907841E-17, -0.7071067811866271757 ) ) ;
#7068 = AXIS2_PLACEMENT_3D ( 'NONE', #3902, #6471, #5845 ) ;
#7069 = PLANE ( 'NONE',  #4355 ) ;
#7070 = FACE_OUTER_BOUND ( 'NONE', #5030, .T. ) ;
#7071 = CARTESIAN_POINT ( 'NONE',  ( 12.49987068959938341, -48.41232521539284051, -12.91614503987825735 ) ) ;
#7072 = CARTESIAN_POINT ( 'NONE',  ( 5.000000000000000000, 4.685197434473814759, -5.637851296924623057E-15 ) ) ;
#7073 = CARTESIAN_POINT ( 'NONE',  ( 75.00000000000000000, 55.00000000000000711, 27.50000000000000000 ) ) ;
#7074 = COLOUR_RGB ( '',0.7921568627450980005, 0.8196078431372548767, 0.9333333333333333481 ) ;
#7075 = EDGE_CURVE ( 'NONE', #426, #1143, #3085, .T. ) ;
#7076 = ORIENTED_EDGE ( 'NONE', *, *, #4358, .F. ) ;
#7077 = EDGE_CURVE ( 'NONE', #3725, #1277, #400, .T. ) ;
#7078 = EDGE_LOOP ( 'NONE', ( #5412, #2701 ) ) ;
#7079 = ORIENTED_EDGE ( 'NONE', *, *, #2474, .F. ) ;
#7080 = PLANE ( 'NONE',  #377 ) ;
#7081 = EDGE_CURVE ( 'NONE', #3598, #6062, #6817, .T. ) ;
#7082 = VERTEX_POINT ( 'NONE', #269 ) ;
#7083 = DIRECTION ( 'NONE',  ( -0.000000000000000000, -0.000000000000000000, 1.000000000000000000 ) ) ;
#7084 = CARTESIAN_POINT ( 'NONE',  ( 0.000000000000000000, -125.0000000000000000, -12.50000000000000000 ) ) ;
#7085 = DIRECTION ( 'NONE',  ( -1.000000000000000000, 0.000000000000000000, 0.000000000000000000 ) ) ;
#7086 = ORIENTED_EDGE ( 'NONE', *, *, #2976, .T. ) ;
#7087 = CONICAL_SURFACE ( 'NONE', #5062, 4.999999999999990230, 1.029744258676653201 ) ;
#7088 = DIRECTION ( 'NONE',  ( 9.992007221626408864E-16, 1.000000000000000000, 0.000000000000000000 ) ) ;
#7089 = ORIENTED_EDGE ( 'NONE', *, *, #3746, .F. ) ;
#7090 = ORIENTED_EDGE ( 'NONE', *, *, #4431, .T. ) ;
#7091 = SURFACE_SIDE_STYLE ('',( #4500 ) ) ;
#7092 = VECTOR ( 'NONE', #5111, 1000.000000000000000 ) ;
#7093 = ORIENTED_EDGE ( 'NONE', *, *, #1803, .F. ) ;
#7094 =( GEOMETRIC_REPRESENTATION_CONTEXT ( 3 ) GLOBAL_UNCERTAINTY_ASSIGNED_CONTEXT ( ( #3110 ) ) GLOBAL_UNIT_ASSIGNED_CONTEXT ( ( #2351, #4819, #2960 ) ) REPRESENTATION_CONTEXT ( 'NONE', 'WORKASPACE' ) );
#7095 = CARTESIAN_POINT ( 'NONE',  ( -4.038684223623520531, 49.84236097863853132, -24.35762614583960683 ) ) ;
#7096 = CIRCLE ( 'NONE', #2031, 4.999999999999990230 ) ;
#7097 = DIRECTION ( 'NONE',  ( -0.000000000000000000, -0.000000000000000000, 1.000000000000000000 ) ) ;
#7098 = DIRECTION ( 'NONE',  ( -1.000000000000000000, -0.000000000000000000, -0.000000000000000000 ) ) ;
#7099 = FACE_OUTER_BOUND ( 'NONE', #7404, .T. ) ;
#7100 = COLOUR_RGB ( '',0.7921568627450980005, 0.8196078431372548767, 0.9333333333333333481 ) ;
#7101 = DIRECTION ( 'NONE',  ( 0.000000000000000000, -1.000000000000000000, 0.000000000000000000 ) ) ;
#7102 = DIRECTION ( 'NONE',  ( -0.000000000000000000, -1.460819769243626884E-16, -1.000000000000000000 ) ) ;
#7103 = ADVANCED_FACE ( 'NONE', ( #3464 ), #4972, .F. ) ;
#7104 = ORIENTED_EDGE ( 'NONE', *, *, #5346, .F. ) ;
#7105 = DIRECTION ( 'NONE',  ( 0.000000000000000000, 0.000000000000000000, -1.000000000000000000 ) ) ;
#7106 = EDGE_CURVE ( 'NONE', #4879, #1112, #5792, .T. ) ;
#7107 = DIRECTION ( 'NONE',  ( -0.1584884973581719703, 6.974650036205672365E-17, -0.9873608237139798183 ) ) ;
#7108 = VERTEX_POINT ( 'NONE', #4262 ) ;
#7109 = VECTOR ( 'NONE', #3732, 1000.000000000000000 ) ;
#7110 = VERTEX_POINT ( 'NONE', #8088 ) ;
#7111 = LINE ( 'NONE', #3939, #907 ) ;
#7112 = CIRCLE ( 'NONE', #356, 20.00000000000000355 ) ;
#7113 = FACE_OUTER_BOUND ( 'NONE', #2468, .T. ) ;
#7114 = ADVANCED_FACE ( 'NONE', ( #2317 ), #6863, .F. ) ;
#7115 = ADVANCED_FACE ( 'NONE', ( #5518 ), #1672, .F. ) ;
#7116 = CARTESIAN_POINT ( 'NONE',  ( 10.84905357516155888, -48.81101040073316710, -6.237423197851056145 ) ) ;
#7117 = DIRECTION ( 'NONE',  ( 1.000000000000000000, 0.000000000000000000, 0.000000000000000000 ) ) ;
#7118 = AXIS2_PLACEMENT_3D ( 'NONE', #3556, #919, #6659 ) ;
#7119 = DIRECTION ( 'NONE',  ( -1.000000000000000000, -0.000000000000000000, -0.000000000000000000 ) ) ;
#7120 = VERTEX_POINT ( 'NONE', #3010 ) ;
#7121 = AXIS2_PLACEMENT_3D ( 'NONE', #7180, #941, #1527 ) ;
#7122 = EDGE_LOOP ( 'NONE', ( #1630, #7902, #368, #1355 ) ) ;
#7123 = CIRCLE ( 'NONE', #4813, 4.057500000000000107 ) ;
#7124 = EDGE_LOOP ( 'NONE', ( #7755, #2463, #7658, #3616 ) ) ;
#7125 = LINE ( 'NONE', #6526, #7679 ) ;
#7126 = VERTEX_POINT ( 'NONE', #5599 ) ;
#7127 = CARTESIAN_POINT ( 'NONE',  ( 0.000000000000000000, 0.000000000000000000, 0.000000000000000000 ) ) ;
#7128 = DIRECTION ( 'NONE',  ( -0.8571673007021112234, 1.049727191138617340E-16, 0.5150380749100560429 ) ) ;
#7129 = VECTOR ( 'NONE', #4595, 1000.000000000000000 ) ;
#7130 = CIRCLE ( 'NONE', #6582, 20.00000000000000355 ) ;
#7131 = CARTESIAN_POINT ( 'NONE',  ( 55.00000000000000000, -55.00000000000000000, 220.0000000000000284 ) ) ;
#7132 = VECTOR ( 'NONE', #5180, 1000.000000000000000 ) ;
#7133 = VECTOR ( 'NONE', #4747, 1000.000000000000000 ) ;
#7134 = DIRECTION ( 'NONE',  ( 0.000000000000000000, 1.000000000000000000, 0.000000000000000000 ) ) ;
#7135 = ORIENTED_EDGE ( 'NONE', *, *, #4420, .T. ) ;
#7136 = FACE_OUTER_BOUND ( 'NONE', #7721, .T. ) ;
#7137 = EDGE_CURVE ( 'NONE', #8125, #1878, #8176, .T. ) ;
#7138 = AXIS2_PLACEMENT_3D ( 'NONE', #7460, #5386, #2198 ) ;
#7139 = DIRECTION ( 'NONE',  ( 0.000000000000000000, 0.000000000000000000, -1.000000000000000000 ) ) ;
#7140 = CARTESIAN_POINT ( 'NONE',  ( 0.000000000000000000, -2.590378953665082788E-32, -3.260250431704825048E-15 ) ) ;
#7141 = ORIENTED_EDGE ( 'NONE', *, *, #3394, .F. ) ;
#7142 = CYLINDRICAL_SURFACE ( 'NONE', #2414, 37.49999999999999289 ) ;
#7143 = AXIS2_PLACEMENT_3D ( 'NONE', #3129, #3043, #1249 ) ;
#7144 = DIRECTION ( 'NONE',  ( 1.000000000000000000, 2.921639538487254261E-16, -0.000000000000000000 ) ) ;
#7145 = CARTESIAN_POINT ( 'NONE',  ( -54.99999999999999289, 75.00000000000000000, -27.50000000000000000 ) ) ;
#7146 = ORIENTED_EDGE ( 'NONE', *, *, #6490, .F. ) ;
#7147 = LINE ( 'NONE', #2787, #5342 ) ;
#7148 = CARTESIAN_POINT ( 'NONE',  ( 115.0000000000000142, 114.9999999999997442, -1.599999999999995426 ) ) ;
#7149 = ORIENTED_EDGE ( 'NONE', *, *, #6476, .T. ) ;
#7150 = ORIENTED_EDGE ( 'NONE', *, *, #7009, .F. ) ;
#7151 = CARTESIAN_POINT ( 'NONE',  ( -54.99999999999999289, 55.00000000000000711, 27.50000000000000000 ) ) ;
#7152 = CARTESIAN_POINT ( 'NONE',  ( 125.0000000000000000, 125.0000000000000000, 340.0000000000000000 ) ) ;
#7153 = DIRECTION ( 'NONE',  ( 0.000000000000000000, 0.000000000000000000, -1.000000000000000000 ) ) ;
#7154 = APPLICATION_CONTEXT ( 'automotive_design' ) ;
#7155 = FACE_OUTER_BOUND ( 'NONE', #2319, .T. ) ;
#7156 =( NAMED_UNIT ( * ) PLANE_ANGLE_UNIT ( ) SI_UNIT ( $, .RADIAN. ) );
#7157 = EDGE_CURVE ( 'NONE', #2948, #8106, #4955, .T. ) ;
#7158 = CARTESIAN_POINT ( 'NONE',  ( -114.9999999999999716, 114.9999999999999858, 20.00000000000000000 ) ) ;
#7159 = VERTEX_POINT ( 'NONE', #2845 ) ;
#7160 = DIRECTION ( 'NONE',  ( -1.000000000000000000, -0.000000000000000000, -0.000000000000000000 ) ) ;
#7161 = EDGE_CURVE ( 'NONE', #314, #952, #5431, .T. ) ;
#7162 = ADVANCED_FACE ( 'NONE', ( #6387 ), #1895, .T. ) ;
#7163 = EDGE_CURVE ( 'NONE', #2019, #5164, #1845, .T. ) ;
#7164 = CIRCLE ( 'NONE', #7027, 15.00000000000000000 ) ;
#7165 = ORIENTED_EDGE ( 'NONE', *, *, #152, .T. ) ;
#7166 = DIRECTION ( 'NONE',  ( -1.000000000000000000, -0.000000000000000000, -0.000000000000000000 ) ) ;
#7167 = EDGE_LOOP ( 'NONE', ( #6957, #5576 ) ) ;
#7168 = CARTESIAN_POINT ( 'NONE',  ( 1.530808498934191521E-15, 125.0000000000000000, 0.000000000000000000 ) ) ;
#7169 = CYLINDRICAL_SURFACE ( 'NONE', #1460, 5.999999999999991118 ) ;
#7170 = CONTEXT_DEPENDENT_SHAPE_REPRESENTATION ( #3050, #4442 ) ;
#7171 = LINE ( 'NONE', #4589, #5549 ) ;
#7172 = EDGE_CURVE ( 'NONE', #4314, #3069, #3217, .T. ) ;
#7173 = DIRECTION ( 'NONE',  ( -1.000000000000000000, -0.000000000000000000, -0.000000000000000000 ) ) ;
#7174 = ORIENTED_EDGE ( 'NONE', *, *, #7578, .T. ) ;
#7175 = DIRECTION ( 'NONE',  ( -1.000000000000000000, -0.000000000000000000, -0.000000000000000000 ) ) ;
#7176 = CARTESIAN_POINT ( 'NONE',  ( 0.000000000000000000, 0.000000000000000000, -126.0000000000000284 ) ) ;
#7177 = CARTESIAN_POINT ( 'NONE',  ( 109.5000000000000142, 114.9999999999999716, 20.00000000000000000 ) ) ;
#7178 = ADVANCED_FACE ( 'NONE', ( #5682 ), #3687, .F. ) ;
#7179 = EDGE_CURVE ( 'NONE', #153, #1207, #3765, .T. ) ;
#7180 = CARTESIAN_POINT ( 'NONE',  ( 0.000000000000000000, 0.000000000000000000, -250.0000000000000000 ) ) ;
#7181 = CARTESIAN_POINT ( 'NONE',  ( 50.00000000000000711, -55.00000000000000000, 220.0000000000000284 ) ) ;
#7182 = CARTESIAN_POINT ( 'NONE',  ( 5.000000000000000000, 4.685197434473814759, -5.637851296924623057E-15 ) ) ;
#7183 = AXIS2_PLACEMENT_3D ( 'NONE', #2325, #4877, #8181 ) ;
#7184 = EDGE_CURVE ( 'NONE', #5389, #6321, #5520, .T. ) ;
#7185 = CARTESIAN_POINT ( 'NONE',  ( 0.000000000000000000, 4.685197434473814759, -5.637851296924623057E-15 ) ) ;
#7186 = CARTESIAN_POINT ( 'NONE',  ( 55.00000000000000000, 55.00000000000000000, 220.0000000000000284 ) ) ;
#7187 = VERTEX_POINT ( 'NONE', #8224 ) ;
#7188 = DIRECTION ( 'NONE',  ( -0.000000000000000000, -0.000000000000000000, 1.000000000000000000 ) ) ;
#7189 = DIRECTION ( 'NONE',  ( 1.224646799147348523E-16, 3.160065852750576588E-30, -1.000000000000000000 ) ) ;
#7190 = DIRECTION ( 'NONE',  ( 1.000000000000000000, 0.000000000000000000, 0.000000000000000000 ) ) ;
#7191 = ORIENTED_EDGE ( 'NONE', *, *, #991, .T. ) ;
#7192 = ORIENTED_EDGE ( 'NONE', *, *, #1968, .T. ) ;
#7193 = FACE_OUTER_BOUND ( 'NONE', #7325, .T. ) ;
#7194 = DIRECTION ( 'NONE',  ( -0.000000000000000000, -0.000000000000000000, 1.000000000000000000 ) ) ;
#7195 = FILL_AREA_STYLE_COLOUR ( '', #7074 ) ;
#7196 = CYLINDRICAL_SURFACE ( 'NONE', #4421, 4.999999999999990230 ) ;
#7197 = LINE ( 'NONE', #3339, #5468 ) ;
#7198 = CARTESIAN_POINT ( 'NONE',  ( -125.0000000000000000, -125.0000000000000284, 0.000000000000000000 ) ) ;
#7199 = CYLINDRICAL_SURFACE ( 'NONE', #1721, 8.999999999999994671 ) ;
#7200 = ORIENTED_EDGE ( 'NONE', *, *, #7340, .T. ) ;
#7201 = CARTESIAN_POINT ( 'NONE',  ( -123.9999999999999716, 114.9999999999999858, 20.00000000000000000 ) ) ;
#7202 = VECTOR ( 'NONE', #199, 1000.000000000000000 ) ;
#7203 = SHAPE_REPRESENTATION ( 'Drive Unit', ( #1299 ), #205 ) ;
#7204 = EDGE_LOOP ( 'NONE', ( #237, #3622, #3829, #8309 ) ) ;
#7205 = CARTESIAN_POINT ( 'NONE',  ( 75.00000000000000000, -54.99999999999999289, -27.50000000000000000 ) ) ;
#7206 = VERTEX_POINT ( 'NONE', #6425 ) ;
#7207 = LINE ( 'NONE', #3351, #4141 ) ;
#7208 = CARTESIAN_POINT ( 'NONE',  ( 114.9999999999999147, -115.0000000000000000, 0.000000000000000000 ) ) ;
#7209 = EDGE_CURVE ( 'NONE', #5533, #5699, #8265, .T. ) ;
#7210 = VECTOR ( 'NONE', #3510, 1000.000000000000000 ) ;
#7211 = ADVANCED_FACE ( 'NONE', ( #5042 ), #657, .T. ) ;
#7212 = DIRECTION ( 'NONE',  ( 0.000000000000000000, 0.000000000000000000, 1.000000000000000000 ) ) ;
#7213 = ORIENTED_EDGE ( 'NONE', *, *, #4254, .T. ) ;
#7214 = DIRECTION ( 'NONE',  ( -0.000000000000000000, -0.000000000000000000, 1.000000000000000000 ) ) ;
#7215 =( REPRESENTATION_RELATIONSHIP ('NONE','NONE', #6882, #239 ) REPRESENTATION_RELATIONSHIP_WITH_TRANSFORMATION ( #4340 )SHAPE_REPRESENTATION_RELATIONSHIP( ) );
#7216 = EDGE_CURVE ( 'NONE', #416, #6212, #1213, .T. ) ;
#7217 = EDGE_CURVE ( 'NONE', #7967, #7126, #1072, .T. ) ;
#7218 = ADVANCED_FACE ( 'NONE', ( #5766 ), #3055, .T. ) ;
#7219 = CARTESIAN_POINT ( 'NONE',  ( -125.0000000000000000, -52.49999999999997158, 0.000000000000000000 ) ) ;
#7220 = DIRECTION ( 'NONE',  ( 1.000000000000000000, 0.000000000000000000, 0.000000000000000000 ) ) ;
#7221 = CYLINDRICAL_SURFACE ( 'NONE', #1597, 4.999999999999997335 ) ;
#7222 = FACE_OUTER_BOUND ( 'NONE', #4315, .T. ) ;
#7223 = CARTESIAN_POINT ( 'NONE',  ( 5.000000000000000000, 2.342598717236915373, 4.057499999999997442 ) ) ;
#7224 = CYLINDRICAL_SURFACE ( 'NONE', #8340, 8.999999999999994671 ) ;
#7225 = AXIS2_PLACEMENT_3D ( 'NONE', #5724, #5044, #4392 ) ;
#7226 = CARTESIAN_POINT ( 'NONE',  ( 95.00000000000000000, 95.00000000000008527, 70.00000000000000000 ) ) ;
#7227 = ORIENTED_EDGE ( 'NONE', *, *, #3331, .T. ) ;
#7228 = LINE ( 'NONE', #168, #7367 ) ;
#7229 = EDGE_CURVE ( 'NONE', #3799, #2674, #5002, .T. ) ;
#7230 = CARTESIAN_POINT ( 'NONE',  ( -114.9999999999999858, 114.9999999999999432, -1.599999999999995426 ) ) ;
#7231 = VERTEX_POINT ( 'NONE', #7589 ) ;
#7232 = CONICAL_SURFACE ( 'NONE', #2393, 4.999999999999990230, 1.029744258676653201 ) ;
#7233 = CARTESIAN_POINT ( 'NONE',  ( -15.00000000000000000, 1.836970198721029589E-15, -28.00000000000002487 ) ) ;
#7234 = CARTESIAN_POINT ( 'NONE',  ( -120.4999999999999858, -114.9999999999999858, 20.00000000000000000 ) ) ;
#7235 = DIRECTION ( 'NONE',  ( 1.000000000000000000, 0.000000000000000000, 0.000000000000000000 ) ) ;
#7236 = DIRECTION ( 'NONE',  ( -0.000000000000000000, -0.000000000000000000, 1.000000000000000000 ) ) ;
#7237 = SURFACE_STYLE_USAGE ( .BOTH. , #7884 ) ;
#7238 = DIRECTION ( 'NONE',  ( 0.000000000000000000, 0.000000000000000000, 1.000000000000000000 ) ) ;
#7239 = AXIS2_PLACEMENT_3D ( 'NONE', #363, #7476, #3561 ) ;
#7240 = DIRECTION ( 'NONE',  ( -0.000000000000000000, -0.000000000000000000, 1.000000000000000000 ) ) ;
#7241 = LINE ( 'NONE', #7768, #1192 ) ;
#7242 = ORIENTED_EDGE ( 'NONE', *, *, #6422, .T. ) ;
#7243 = FACE_OUTER_BOUND ( 'NONE', #435, .T. ) ;
#7244 = AXIS2_PLACEMENT_3D ( 'NONE', #382, #988, #1749 ) ;
#7245 = PLANE ( 'NONE',  #2553 ) ;
#7246 = ORIENTED_EDGE ( 'NONE', *, *, #284, .T. ) ;
#7247 = DIRECTION ( 'NONE',  ( 0.000000000000000000, 0.000000000000000000, 1.000000000000000000 ) ) ;
#7248 = CIRCLE ( 'NONE', #7666, 4.999999999999990230 ) ;
#7249 = EDGE_LOOP ( 'NONE', ( #5424, #5009 ) ) ;
#7250 = CARTESIAN_POINT ( 'NONE',  ( 114.9999999999999147, -115.0000000000000000, 250.0000000000000000 ) ) ;
#7251 = DIRECTION ( 'NONE',  ( -1.000000000000000000, -0.000000000000000000, -0.000000000000000000 ) ) ;
#7252 = AXIS2_PLACEMENT_3D ( 'NONE', #978, #6107, #328 ) ;
#7253 = CARTESIAN_POINT ( 'NONE',  ( 49.00000000000000000, 55.00000000000000711, 27.50000000000000000 ) ) ;
#7254 = CIRCLE ( 'NONE', #364, 57.99999999999995737 ) ;
#7255 = EDGE_CURVE ( 'NONE', #7187, #7585, #1939, .T. ) ;
#7256 = VERTEX_POINT ( 'NONE', #3139 ) ;
#7257 = DIRECTION ( 'NONE',  ( -0.000000000000000000, -0.000000000000000000, 1.000000000000000000 ) ) ;
#7258 = AXIS2_PLACEMENT_3D ( 'NONE', #7901, #886, #4673 ) ;
#7259 = EDGE_LOOP ( 'NONE', ( #7038, #8113, #8027, #6931, #5483, #254, #5269, #6157 ) ) ;
#7260 = DIRECTION ( 'NONE',  ( 1.000000000000000000, 0.000000000000000000, 0.000000000000000000 ) ) ;
#7261 = CIRCLE ( 'NONE', #3887, 15.00000000000000000 ) ;
#7262 = FACE_OUTER_BOUND ( 'NONE', #4922, .T. ) ;
#7263 = EDGE_CURVE ( 'NONE', #3250, #3350, #6723, .T. ) ;
#7264 = VECTOR ( 'NONE', #2536, 1000.000000000000000 ) ;
#7265 = AXIS2_PLACEMENT_3D ( 'NONE', #1905, #1179, #626 ) ;
#7266 = DIRECTION ( 'NONE',  ( 1.000000000000000000, 0.000000000000000000, 0.000000000000000000 ) ) ;
#7267 = ADVANCED_FACE ( 'NONE', ( #7070 ), #2520, .F. ) ;
#7268 = ADVANCED_FACE ( 'NONE', ( #1769 ), #4308, .T. ) ;
#7269 = LINE ( 'NONE', #3322, #3592 ) ;
#7270 = DIRECTION ( 'NONE',  ( -1.000000000000000000, 0.000000000000000000, 0.000000000000000000 ) ) ;
#7271 = FACE_OUTER_BOUND ( 'NONE', #6438, .T. ) ;
#7272 = VECTOR ( 'NONE', #4479, 1000.000000000000000 ) ;
#7273 = CARTESIAN_POINT ( 'NONE',  ( 125.0000000000000000, 125.0000000000000284, 70.00000000000000000 ) ) ;
#7274 = AXIS2_PLACEMENT_3D ( 'NONE', #7909, #2708, #6030 ) ;
#7275 = DIRECTION ( 'NONE',  ( 1.000000000000000000, 0.000000000000000000, 0.000000000000000000 ) ) ;
#7276 = VERTEX_POINT ( 'NONE', #828 ) ;
#7277 = CARTESIAN_POINT ( 'NONE',  ( 114.9999999999999147, 0.000000000000000000, 250.0000000000000000 ) ) ;
#7278 = CARTESIAN_POINT ( 'NONE',  ( -75.00000000000000000, -75.00000000000000000, 27.50000000000000000 ) ) ;
#7279 = CIRCLE ( 'NONE', #3618, 95.00000000000008527 ) ;
#7280 = ORIENTED_EDGE ( 'NONE', *, *, #1024, .T. ) ;
#7281 = VECTOR ( 'NONE', #3479, 1000.000000000000000 ) ;
#7282 = DIRECTION ( 'NONE',  ( -0.000000000000000000, -0.000000000000000000, -1.000000000000000000 ) ) ;
#7283 = FACE_BOUND ( 'NONE', #312, .T. ) ;
#7284 = FACE_OUTER_BOUND ( 'NONE', #8223, .T. ) ;
#7285 = DIRECTION ( 'NONE',  ( 1.000000000000000000, 0.000000000000000000, 0.000000000000000000 ) ) ;
#7286 = DIRECTION ( 'NONE',  ( 0.000000000000000000, 0.000000000000000000, -1.000000000000000000 ) ) ;
#7287 = VECTOR ( 'NONE', #4604, 1000.000000000000000 ) ;
#7288 = CARTESIAN_POINT ( 'NONE',  ( 5.000000000000000000, -2.342598717236898054, 4.057500000000003659 ) ) ;
#7289 = CARTESIAN_POINT ( 'NONE',  ( 10.40000000000000036, 6.123233995736809670E-16, -5.000000000000035527 ) ) ;
#7290 = ORIENTED_EDGE ( 'NONE', *, *, #2196, .T. ) ;
#7291 = DIRECTION ( 'NONE',  ( -0.000000000000000000, -0.000000000000000000, 1.000000000000000000 ) ) ;
#7292 = ADVANCED_FACE ( 'NONE', ( #7155 ), #7196, .F. ) ;
#7293 = DIRECTION ( 'NONE',  ( 0.000000000000000000, -1.000000000000000000, 0.000000000000000000 ) ) ;
#7294 = CARTESIAN_POINT ( 'NONE',  ( -55.00000000000000000, 55.00000000000000000, 220.0000000000000284 ) ) ;
#7295 = ORIENTED_EDGE ( 'NONE', *, *, #5940, .F. ) ;
#7296 = FACE_OUTER_BOUND ( 'NONE', #3589, .T. ) ;
#7297 = CARTESIAN_POINT ( 'NONE',  ( -94.99999999999997158, -95.00000000000008527, 70.00000000000000000 ) ) ;
#7298 = DIRECTION ( 'NONE',  ( -0.000000000000000000, -0.000000000000000000, -1.000000000000000000 ) ) ;
#7299 = DIRECTION ( 'NONE',  ( -0.000000000000000000, -0.000000000000000000, 1.000000000000000000 ) ) ;
#7300 = VECTOR ( 'NONE', #2539, 1000.000000000000000 ) ;
#7301 = ORIENTED_EDGE ( 'NONE', *, *, #4151, .F. ) ;
#7302 = CARTESIAN_POINT ( 'NONE',  ( 20.76917701662883076, 5.000000000000000000, 0.000000000000000000 ) ) ;
#7303 = ORIENTED_EDGE ( 'NONE', *, *, #7448, .T. ) ;
#7304 = SURFACE_SIDE_STYLE ('',( #2096 ) ) ;
#7305 = LINE ( 'NONE', #6669, #5508 ) ;
#7306 = DIRECTION ( 'NONE',  ( -0.000000000000000000, -1.000000000000000000, 1.586032892321652236E-16 ) ) ;
#7307 = FACE_OUTER_BOUND ( 'NONE', #5613, .T. ) ;
#7308 = DIRECTION ( 'NONE',  ( -0.000000000000000000, -0.000000000000000000, 1.000000000000000000 ) ) ;
#7309 = CARTESIAN_POINT ( 'NONE',  ( -31.74999999999995737, 0.000000000000000000, 8.000000000000000000 ) ) ;
#7310 = CARTESIAN_POINT ( 'NONE',  ( 0.000000000000000000, 49.99999999999998579, -100.0000000000000000 ) ) ;
#7311 = CIRCLE ( 'NONE', #2730, 5.000000000000070166 ) ;
#7312 = ORIENTED_EDGE ( 'NONE', *, *, #461, .F. ) ;
#7313 = DIRECTION ( 'NONE',  ( -0.000000000000000000, 0.000000000000000000, 1.000000000000000000 ) ) ;
#7314 = ADVANCED_FACE ( 'NONE', ( #4655 ), #1378, .F. ) ;
#7315 = EDGE_LOOP ( 'NONE', ( #4962, #5122, #1297, #2758 ) ) ;
#7316 = AXIS2_PLACEMENT_3D ( 'NONE', #6295, #1840, #2176 ) ;
#7317 = CARTESIAN_POINT ( 'NONE',  ( 125.0000000000000000, -125.0000000000000284, 70.00000000000000000 ) ) ;
#7318 =( GEOMETRIC_REPRESENTATION_CONTEXT ( 3 ) GLOBAL_UNCERTAINTY_ASSIGNED_CONTEXT ( ( #584 ) ) GLOBAL_UNIT_ASSIGNED_CONTEXT ( ( #5485, #1410, #2855 ) ) REPRESENTATION_CONTEXT ( 'NONE', 'WORKASPACE' ) );
#7319 = SURFACE_STYLE_FILL_AREA ( #4738 ) ;
#7320 = DIRECTION ( 'NONE',  ( 1.000000000000000000, 0.000000000000000000, 0.000000000000000000 ) ) ;
#7321 = DIRECTION ( 'NONE',  ( 1.000000000000000000, 0.000000000000000000, 0.000000000000000000 ) ) ;
#7322 =( NAMED_UNIT ( * ) SI_UNIT ( $, .STERADIAN. ) SOLID_ANGLE_UNIT ( ) );
#7323 = EDGE_CURVE ( 'NONE', #6239, #3602, #802, .T. ) ;
#7324 = SURFACE_STYLE_FILL_AREA ( #7366 ) ;
#7325 = EDGE_LOOP ( 'NONE', ( #5547, #963, #6247 ) ) ;
#7326 = CARTESIAN_POINT ( 'NONE',  ( -114.9999999999999858, -114.9999999999999858, 0.000000000000000000 ) ) ;
#7327 = VERTEX_POINT ( 'NONE', #6516 ) ;
#7328 = DIRECTION ( 'NONE',  ( 1.000000000000000000, 0.000000000000000000, 0.000000000000000000 ) ) ;
#7329 = AXIS2_PLACEMENT_3D ( 'NONE', #161, #2741, #4764 ) ;
#7330 = DIRECTION ( 'NONE',  ( 0.000000000000000000, 0.000000000000000000, 1.000000000000000000 ) ) ;
#7331 = ORIENTED_EDGE ( 'NONE', *, *, #4733, .T. ) ;
#7332 = ORIENTED_EDGE ( 'NONE', *, *, #4536, .T. ) ;
#7333 = DIRECTION ( 'NONE',  ( 1.000000000000000000, 0.000000000000000000, 0.000000000000000000 ) ) ;
#7334 = CARTESIAN_POINT ( 'NONE',  ( -125.0000000000002558, -125.0000000000000000, 0.000000000000000000 ) ) ;
#7335 = ITEM_DEFINED_TRANSFORMATION ( 'NONE', 'NONE', #2609,  #1299 ) ;
#7336 = ADVANCED_FACE ( 'NONE', ( #2684 ), #4055, .F. ) ;
#7337 = DIRECTION ( 'NONE',  ( 1.000000000000000000, 0.000000000000000000, 0.000000000000000000 ) ) ;
#7338 = CYLINDRICAL_SURFACE ( 'NONE', #2593, 5.999999999999991118 ) ;
#7339 = AXIS2_PLACEMENT_3D ( 'NONE', #3505, #313, #4665 ) ;
#7340 = EDGE_CURVE ( 'NONE', #351, #3120, #5926, .T. ) ;
#7341 = PRODUCT_DEFINITION_CONTEXT ( 'detailed design', #6561, 'design' ) ;
#7342 = ORIENTED_EDGE ( 'NONE', *, *, #6024, .F. ) ;
#7343 = DIRECTION ( 'NONE',  ( 0.000000000000000000, 1.000000000000000000, 0.000000000000000000 ) ) ;
#7344 = ORIENTED_EDGE ( 'NONE', *, *, #2429, .T. ) ;
#7345 =( NAMED_UNIT ( * ) SI_UNIT ( $, .STERADIAN. ) SOLID_ANGLE_UNIT ( ) );
#7346 = AXIS2_PLACEMENT_3D ( 'NONE', #2250, #3469, #4832 ) ;
#7347 = ORIENTED_EDGE ( 'NONE', *, *, #1343, .F. ) ;
#7348 = CARTESIAN_POINT ( 'NONE',  ( -75.00000000000000000, -75.00000000000000000, 27.50000000000000000 ) ) ;
#7349 = CARTESIAN_POINT ( 'NONE',  ( -123.9999999999999716, 114.9999999999999858, 20.00000000000000000 ) ) ;
#7350 = CARTESIAN_POINT ( 'NONE',  ( 120.0000000000000000, 115.0000000000000000, 340.0000000000000000 ) ) ;
#7351 = DIRECTION ( 'NONE',  ( 0.000000000000000000, 0.000000000000000000, -1.000000000000000000 ) ) ;
#7352 = DIRECTION ( 'NONE',  ( 0.000000000000000000, 0.000000000000000000, 1.000000000000000000 ) ) ;
#7353 = CARTESIAN_POINT ( 'NONE',  ( 115.0000000000000000, -114.9999999999999716, 20.00000000000000000 ) ) ;
#7354 = FACE_OUTER_BOUND ( 'NONE', #2888, .T. ) ;
#7355=STYLED_ITEM('',(#8407),#950);
#7356 = FACE_OUTER_BOUND ( 'NONE', #7592, .T. ) ;
#7357 = ORIENTED_EDGE ( 'NONE', *, *, #8312, .T. ) ;
#7358 = EDGE_LOOP ( 'NONE', ( #750, #4342, #2161 ) ) ;
#7359 = LINE ( 'NONE', #6403, #5961 ) ;
#7360 = CARTESIAN_POINT ( 'NONE',  ( 0.000000000000000000, 0.000000000000000000, 0.000000000000000000 ) ) ;
#7361 = AXIS2_PLACEMENT_3D ( 'NONE', #6441, #675, #6362 ) ;
#7362 = EDGE_CURVE ( 'NONE', #8240, #1008, #3338, .T. ) ;
#7363 = CARTESIAN_POINT ( 'NONE',  ( 0.000000000000000000, 0.000000000000000000, -128.0000000000000284 ) ) ;
#7364 = DIRECTION ( 'NONE',  ( 0.000000000000000000, 0.000000000000000000, 1.000000000000000000 ) ) ;
#7365 = CARTESIAN_POINT ( 'NONE',  ( -11.86014387961075833, -48.57408496170467771, -16.53260109561407276 ) ) ;
#7366 = FILL_AREA_STYLE ('',( #4742 ) ) ;
#7367 = VECTOR ( 'NONE', #2020, 1000.000000000000000 ) ;
#7368 = DIRECTION ( 'NONE',  ( -0.000000000000000000, -0.000000000000000000, 1.000000000000000000 ) ) ;
#7369 = VERTEX_POINT ( 'NONE', #865 ) ;
#7370 = AXIS2_PLACEMENT_3D ( 'NONE', #8177, #1090, #1002 ) ;
#7371 = DIRECTION ( 'NONE',  ( 0.000000000000000000, -1.000000000000000000, -1.460819769243626884E-16 ) ) ;
#7372 = EDGE_CURVE ( 'NONE', #952, #1918, #4017, .T. ) ;
#7373 = ADVANCED_FACE ( 'NONE', ( #743 ), #6562, .F. ) ;
#7374 = DIRECTION ( 'NONE',  ( -0.000000000000000000, -0.000000000000000000, 1.000000000000000000 ) ) ;
#7375 = CIRCLE ( 'NONE', #639, 54.99999999999996447 ) ;
#7376 = ORIENTED_EDGE ( 'NONE', *, *, #2164, .F. ) ;
#7377 = CARTESIAN_POINT ( 'NONE',  ( 10.00000000000000000, -3.448762466456902719E-14, 93.74999999999998579 ) ) ;
#7378 = CYLINDRICAL_SURFACE ( 'NONE', #6712, 8.999999999999994671 ) ;
#7379 = ITEM_DEFINED_TRANSFORMATION ( 'NONE', 'NONE', #1944,  #1299 ) ;
#7380 = DIRECTION ( 'NONE',  ( -1.000000000000000000, -0.000000000000000000, -0.000000000000000000 ) ) ;
#7381 = CARTESIAN_POINT ( 'NONE',  ( -114.9999999999999716, 114.9999999999999858, 20.00000000000000000 ) ) ;
#7382 =( REPRESENTATION_RELATIONSHIP ('NONE','NONE', #6882, #1708 ) REPRESENTATION_RELATIONSHIP_WITH_TRANSFORMATION ( #4588 )SHAPE_REPRESENTATION_RELATIONSHIP( ) );
#7383 = VECTOR ( 'NONE', #6412, 1000.000000000000000 ) ;
#7384 = VECTOR ( 'NONE', #3863, 1000.000000000000000 ) ;
#7385 = VERTEX_POINT ( 'NONE', #213 ) ;
#7386 = DIRECTION ( 'NONE',  ( 1.000000000000000000, 0.000000000000000000, 0.000000000000000000 ) ) ;
#7387 = ORIENTED_EDGE ( 'NONE', *, *, #4023, .F. ) ;
#7388 = DIRECTION ( 'NONE',  ( 0.000000000000000000, -2.960594732333750117E-16, 1.000000000000000000 ) ) ;
#7389 = AXIS2_PLACEMENT_3D ( 'NONE', #7021, #730, #7619 ) ;
#7390 = DIRECTION ( 'NONE',  ( 0.000000000000000000, 0.000000000000000000, -1.000000000000000000 ) ) ;
#7391 = CONICAL_SURFACE ( 'NONE', #1877, 4.999999999999990230, 1.029744258676653201 ) ;
#7392 = ORIENTED_EDGE ( 'NONE', *, *, #4091, .T. ) ;
#7393 = CARTESIAN_POINT ( 'NONE',  ( 7.620025376658134952, 49.41698073774414013, -2.582688914155140125 ) ) ;
#7394 = EDGE_CURVE ( 'NONE', #7579, #5443, #6331, .T. ) ;
#7395 = DIRECTION ( 'NONE',  ( 0.000000000000000000, -1.000000000000000000, 0.000000000000000000 ) ) ;
#7396 = CIRCLE ( 'NONE', #371, 5.999999999999991118 ) ;
#7397 = DIRECTION ( 'NONE',  ( -0.000000000000000000, -7.945337353457666666E-18, -1.000000000000000000 ) ) ;
#7398 = LINE ( 'NONE', #1615, #3098 ) ;
#7399 = EDGE_LOOP ( 'NONE', ( #294, #4033, #492 ) ) ;
#7400 =( NAMED_UNIT ( * ) PLANE_ANGLE_UNIT ( ) SI_UNIT ( $, .RADIAN. ) );
#7401 = AXIS2_PLACEMENT_3D ( 'NONE', #3871, #3832, #8318 ) ;
#7402 = CIRCLE ( 'NONE', #656, 0.4000000000000001887 ) ;
#7403 = EDGE_LOOP ( 'NONE', ( #2150, #2985, #7086, #4755 ) ) ;
#7404 = EDGE_LOOP ( 'NONE', ( #6087, #5061, #6158, #1501 ) ) ;
#7405 = ORIENTED_EDGE ( 'NONE', *, *, #396, .F. ) ;
#7406 = LINE ( 'NONE', #337, #7518 ) ;
#7407 = AXIS2_PLACEMENT_3D ( 'NONE', #4910, #4870, #1042 ) ;
#7408 = AXIS2_PLACEMENT_3D ( 'NONE', #1713, #6051, #7330 ) ;
#7409 = DIRECTION ( 'NONE',  ( -0.000000000000000000, -7.945337353457666666E-18, -1.000000000000000000 ) ) ;
#7410 = DIRECTION ( 'NONE',  ( 0.000000000000000000, 0.000000000000000000, 1.000000000000000000 ) ) ;
#7411 = ORIENTED_EDGE ( 'NONE', *, *, #2649, .T. ) ;
#7412 = FACE_OUTER_BOUND ( 'NONE', #8234, .T. ) ;
#7413 = AXIS2_PLACEMENT_3D ( 'NONE', #5211, #7236, #6608 ) ;
#7414 = CIRCLE ( 'NONE', #7138, 5.499999999999991118 ) ;
#7415 = CARTESIAN_POINT ( 'NONE',  ( -114.9999999999999716, 114.9999999999999858, 20.00000000000000000 ) ) ;
#7416 = VERTEX_POINT ( 'NONE', #3412 ) ;
#7417 = DIRECTION ( 'NONE',  ( 1.000000000000000000, 1.460819769243625652E-16, -0.000000000000000000 ) ) ;
#7418 = CIRCLE ( 'NONE', #119, 75.00000000000001421 ) ;
#7419 = ORIENTED_EDGE ( 'NONE', *, *, #917, .T. ) ;
#7420 = CONICAL_SURFACE ( 'NONE', #1622, 4.999999999999990230, 1.029744258676656754 ) ;
#7421 = ORIENTED_EDGE ( 'NONE', *, *, #3851, .T. ) ;
#7422 = CARTESIAN_POINT ( 'NONE',  ( 114.9999999999999147, -115.0000000000000000, -28.00000000000002487 ) ) ;
#7423 = DIRECTION ( 'NONE',  ( -0.000000000000000000, -0.000000000000000000, 1.000000000000000000 ) ) ;
#7424 = PRODUCT_RELATED_PRODUCT_CATEGORY ( 'part', '', ( #7427 ) ) ;
#7425 = ORIENTED_EDGE ( 'NONE', *, *, #3367, .T. ) ;
#7426 = CYLINDRICAL_SURFACE ( 'NONE', #873, 5.499999999999991118 ) ;
#7427 = PRODUCT ( 'socket head cap screw_am_B18.3.1M - 10 x 1.5 x 70 Hex SHCS -- 32NHX', 'socket head cap screw_am_B18.3.1M - 10 x 1.5 x 70 Hex SHCS -- 32NHX', '', ( #6925 ) ) ;
#7428 = DIRECTION ( 'NONE',  ( -1.460819769243626145E-16, 1.000000000000000000, 0.000000000000000000 ) ) ;
#7429 = EDGE_CURVE ( 'NONE', #5749, #6477, #784, .T. ) ;
#7430 = PRODUCT_DEFINITION_CONTEXT ( 'detailed design', #299, 'design' ) ;
#7431 = ORIENTED_EDGE ( 'NONE', *, *, #5515, .T. ) ;
#7432 = DIRECTION ( 'NONE',  ( 0.000000000000000000, 0.000000000000000000, -1.000000000000000000 ) ) ;
#7433 = ORIENTED_EDGE ( 'NONE', *, *, #7216, .F. ) ;
#7434 = PLANE ( 'NONE',  #7940 ) ;
#7435 = APPLICATION_CONTEXT ( 'automotive_design' ) ;
#7436 = EDGE_LOOP ( 'NONE', ( #6900, #3709 ) ) ;
#7437 = DIRECTION ( 'NONE',  ( 1.000000000000000000, 0.000000000000000000, 0.000000000000000000 ) ) ;
#7438 = ADVANCED_FACE ( 'NONE', ( #7113 ), #4612, .F. ) ;
#7439 = EDGE_CURVE ( 'NONE', #4076, #8191, #2818, .T. ) ;
#7440 = DIRECTION ( 'NONE',  ( -0.000000000000000000, -0.000000000000000000, 1.000000000000000000 ) ) ;
#7441 = CARTESIAN_POINT ( 'NONE',  ( 9.999999999999994671, 0.000000000000000000, 0.000000000000000000 ) ) ;
#7442 = CIRCLE ( 'NONE', #9, 4.999999999999997335 ) ;
#7443 = ORIENTED_EDGE ( 'NONE', *, *, #4836, .F. ) ;
#7444 = DIRECTION ( 'NONE',  ( -0.000000000000000000, -0.000000000000000000, 1.000000000000000000 ) ) ;
#7445 = EDGE_LOOP ( 'NONE', ( #6973, #1906 ) ) ;
#7446 = ORIENTED_EDGE ( 'NONE', *, *, #6378, .T. ) ;
#7447 = ADVANCED_FACE ( 'NONE', ( #7917 ), #3903, .T. ) ;
#7448 = EDGE_CURVE ( 'NONE', #6887, #2803, #4520, .T. ) ;
#7449 = VERTEX_POINT ( 'NONE', #701 ) ;
#7450 = DIRECTION ( 'NONE',  ( -0.000000000000000000, -0.000000000000000000, 1.000000000000000000 ) ) ;
#7451 = VERTEX_POINT ( 'NONE', #3257 ) ;
#7452 = DIRECTION ( 'NONE',  ( 1.000000000000000000, 0.000000000000000000, 0.000000000000000000 ) ) ;
#7453 = CARTESIAN_POINT ( 'NONE',  ( 102.5000000000000000, 0.000000000000000000, 9.499999999999952038 ) ) ;
#7454 = ORIENTED_EDGE ( 'NONE', *, *, #1462, .T. ) ;
#7455 = CARTESIAN_POINT ( 'NONE',  ( -12.17797428566710316, -48.49436920628652103, -9.651054563031587819 ) ) ;
#7456 = CIRCLE ( 'NONE', #7593, 5.999999999999984901 ) ;
#7457 = ORIENTED_EDGE ( 'NONE', *, *, #512, .T. ) ;
#7458 = DIRECTION ( 'NONE',  ( -0.000000000000000000, -0.000000000000000000, 1.000000000000000000 ) ) ;
#7459 = DIRECTION ( 'NONE',  ( -0.000000000000000000, -0.000000000000000000, 1.000000000000000000 ) ) ;
#7460 = CARTESIAN_POINT ( 'NONE',  ( 115.0000000000000000, -114.9999999999999716, 0.000000000000000000 ) ) ;
#7461 = DIRECTION ( 'NONE',  ( -0.000000000000000000, -0.000000000000000000, 1.000000000000000000 ) ) ;
#7462 = CARTESIAN_POINT ( 'NONE',  ( 54.99999999999999289, -54.99999999999999289, 27.50000000000000000 ) ) ;
#7463 =( GEOMETRIC_REPRESENTATION_CONTEXT ( 3 ) GLOBAL_UNCERTAINTY_ASSIGNED_CONTEXT ( ( #1855 ) ) GLOBAL_UNIT_ASSIGNED_CONTEXT ( ( #3540, #6120, #342 ) ) REPRESENTATION_CONTEXT ( 'NONE', 'WORKASPACE' ) );
#7464 = CARTESIAN_POINT ( 'NONE',  ( 10.00000000000000000, -55.00000000000000711, 93.74999999999998579 ) ) ;
#7465 = CARTESIAN_POINT ( 'NONE',  ( 1.530808498934191521E-15, 125.0000000000000000, 0.000000000000000000 ) ) ;
#7466 = CARTESIAN_POINT ( 'NONE',  ( -75.00000000000000000, -54.99999999999999289, 27.50000000000000000 ) ) ;
#7467 = ORIENTED_EDGE ( 'NONE', *, *, #1759, .T. ) ;
#7468 = ORIENTED_EDGE ( 'NONE', *, *, #5159, .T. ) ;
#7469 = DIRECTION ( 'NONE',  ( 0.000000000000000000, 0.000000000000000000, -1.000000000000000000 ) ) ;
#7470 = ORIENTED_EDGE ( 'NONE', *, *, #6036, .T. ) ;
#7471 = ADVANCED_FACE ( 'NONE', ( #2029 ), #6166, .F. ) ;
#7472 = CARTESIAN_POINT ( 'NONE',  ( 6.314393452555577824E-14, 12.50000000000001066, 12.49999999999997868 ) ) ;
#7473 = EDGE_LOOP ( 'NONE', ( #8077, #7003 ) ) ;
#7474 = AXIS2_PLACEMENT_3D ( 'NONE', #6591, #5287, #768 ) ;
#7475 = PRODUCT_CONTEXT ( 'NONE', #5860, 'mechanical' ) ;
#7476 = DIRECTION ( 'NONE',  ( -0.000000000000000000, -0.000000000000000000, 1.000000000000000000 ) ) ;
#7477 = ORIENTED_EDGE ( 'NONE', *, *, #7944, .T. ) ;
#7478 = LINE ( 'NONE', #6023, #3914 ) ;
#7479 = VERTEX_POINT ( 'NONE', #992 ) ;
#7480 = ADVANCED_FACE ( 'NONE', ( #8076 ), #3536, .F. ) ;
#7481 = ORIENTED_EDGE ( 'NONE', *, *, #7484, .T. ) ;
#7482 = AXIS2_PLACEMENT_3D ( 'NONE', #2494, #4882, #451 ) ;
#7483 = CARTESIAN_POINT ( 'NONE',  ( -1.110223024625156540E-13, -12.49999999999999645, 1.387778780781445676E-14 ) ) ;
#7484 = EDGE_CURVE ( 'NONE', #3350, #8314, #4134, .T. ) ;
#7485 = DIRECTION ( 'NONE',  ( 0.000000000000000000, 1.000000000000000000, 0.000000000000000000 ) ) ;
#7486 = ADVANCED_FACE ( 'NONE', ( #6808 ), #807, .T. ) ;
#7487 = VERTEX_POINT ( 'NONE', #2795 ) ;
#7488 = ORIENTED_EDGE ( 'NONE', *, *, #4211, .F. ) ;
#7489 = AXIS2_PLACEMENT_3D ( 'NONE', #6767, #7240, #831 ) ;
#7490 = EDGE_LOOP ( 'NONE', ( #1648, #7498 ) ) ;
#7491 = CARTESIAN_POINT ( 'NONE',  ( -114.9999999999999147, 99.99999999999998579, 250.0000000000000000 ) ) ;
#7492 = EDGE_CURVE ( 'NONE', #984, #4671, #7279, .T. ) ;
#7493 = DIRECTION ( 'NONE',  ( 0.000000000000000000, 0.000000000000000000, 1.000000000000000000 ) ) ;
#7494 = CARTESIAN_POINT ( 'NONE',  ( -12.50034226774478441, -48.41220345444931183, -13.31371842734951727 ) ) ;
#7495 = ORIENTED_EDGE ( 'NONE', *, *, #7944, .F. ) ;
#7496 = CARTESIAN_POINT ( 'NONE',  ( 115.0000000000000000, 114.9999999999999716, 0.000000000000000000 ) ) ;
#7497 = DIRECTION ( 'NONE',  ( -0.000000000000000000, -0.000000000000000000, 1.000000000000000000 ) ) ;
#7498 = ORIENTED_EDGE ( 'NONE', *, *, #6138, .F. ) ;
#7499 = DIRECTION ( 'NONE',  ( -0.000000000000000000, -0.000000000000000000, 1.000000000000000000 ) ) ;
#7500 = CARTESIAN_POINT ( 'NONE',  ( 3.257004588345654206, -49.90043368416228731, -24.59660869042692966 ) ) ;
#7501 = CYLINDRICAL_SURFACE ( 'NONE', #5847, 2.499999999999990230 ) ;
#7502 = CARTESIAN_POINT ( 'NONE',  ( 5.000000000000000000, 7.027796151710712813, -4.057500000000006324 ) ) ;
#7503 = ORIENTED_EDGE ( 'NONE', *, *, #1647, .T. ) ;
#7504 = CIRCLE ( 'NONE', #3047, 12.99999999999999822 ) ;
#7505 = ORIENTED_EDGE ( 'NONE', *, *, #7851, .F. ) ;
#7506 = DIRECTION ( 'NONE',  ( 0.000000000000000000, 0.000000000000000000, 1.000000000000000000 ) ) ;
#7507 = ORIENTED_EDGE ( 'NONE', *, *, #4358, .T. ) ;
#7508 = DIRECTION ( 'NONE',  ( -1.000000000000000000, 0.000000000000000000, 0.000000000000000000 ) ) ;
#7509 = DIRECTION ( 'NONE',  ( 1.000000000000000000, 0.000000000000000000, 0.000000000000000000 ) ) ;
#7510 = ORIENTED_EDGE ( 'NONE', *, *, #3641, .T. ) ;
#7511 = PRODUCT_CONTEXT ( 'NONE', #7867, 'mechanical' ) ;
#7512 = VECTOR ( 'NONE', #436, 1000.000000000000000 ) ;
#7513 = ORIENTED_EDGE ( 'NONE', *, *, #6547, .F. ) ;
#7514 = DIRECTION ( 'NONE',  ( 0.000000000000000000, 0.000000000000000000, 1.000000000000000000 ) ) ;
#7515 = EDGE_CURVE ( 'NONE', #7206, #3094, #1661, .T. ) ;
#7516 = EDGE_LOOP ( 'NONE', ( #6879, #2374, #6873, #7539 ) ) ;
#7517 = DIRECTION ( 'NONE',  ( -1.000000000000000000, 0.000000000000000000, 0.000000000000000000 ) ) ;
#7518 = VECTOR ( 'NONE', #1623, 1000.000000000000000 ) ;
#7519 = ORIENTED_EDGE ( 'NONE', *, *, #6952, .F. ) ;
#7520 = ORIENTED_EDGE ( 'NONE', *, *, #4582, .T. ) ;
#7521 = CARTESIAN_POINT ( 'NONE',  ( 0.000000000000000000, 0.000000000000000000, 0.000000000000000000 ) ) ;
#7522 = FACE_OUTER_BOUND ( 'NONE', #843, .T. ) ;
#7523 = AXIS2_PLACEMENT_3D ( 'NONE', #178, #5422, #6048 ) ;
#7524 = VERTEX_POINT ( 'NONE', #3453 ) ;
#7525 = ORIENTED_EDGE ( 'NONE', *, *, #286, .F. ) ;
#7526 = VECTOR ( 'NONE', #7753, 1000.000000000000000 ) ;
#7527 = DIRECTION ( 'NONE',  ( 0.000000000000000000, 0.000000000000000000, -1.000000000000000000 ) ) ;
#7528 = EDGE_CURVE ( 'NONE', #2097, #860, #8079, .T. ) ;
#7529 = EDGE_CURVE ( 'NONE', #1904, #6580, #2349, .T. ) ;
#7530 = EDGE_CURVE ( 'NONE', #5627, #8339, #5505, .T. ) ;
#7531 = VECTOR ( 'NONE', #5432, 1000.000000000000000 ) ;
#7532 = CARTESIAN_POINT ( 'NONE',  ( 10.00000000000000000, -55.00000000000000711, 93.74999999999998579 ) ) ;
#7533 = CIRCLE ( 'NONE', #3600, 8.999999999999994671 ) ;
#7534 = DIRECTION ( 'NONE',  ( 1.460819769243626145E-16, -1.000000000000000000, 0.000000000000000000 ) ) ;
#7535 = ORIENTED_EDGE ( 'NONE', *, *, #3189, .T. ) ;
#7536 = PRESENTATION_STYLE_ASSIGNMENT (( #6213 ) ) ;
#7537 = SHAPE_REPRESENTATION_RELATIONSHIP ( 'NONE' , 'NONE' ,  #1708, #891 ) ;
#7538 = AXIS2_PLACEMENT_3D ( 'NONE', #7176, #2058, #196 ) ;
#7539 = ORIENTED_EDGE ( 'NONE', *, *, #615, .F. ) ;
#7540 = EDGE_CURVE ( 'NONE', #5777, #5293, #5665, .T. ) ;
#7541 = VERTEX_POINT ( 'NONE', #4739 ) ;
#7542 = VECTOR ( 'NONE', #5138, 1000.000000000000000 ) ;
#7543 = VECTOR ( 'NONE', #1138, 1000.000000000000114 ) ;
#7544 = CARTESIAN_POINT ( 'NONE',  ( -114.9999999999999147, 115.0000000000000000, 0.000000000000000000 ) ) ;
#7545 = DIRECTION ( 'NONE',  ( -1.000000000000000000, 0.000000000000000000, -0.000000000000000000 ) ) ;
#7546 = ORIENTED_EDGE ( 'NONE', *, *, #3253, .F. ) ;
#7547 = CARTESIAN_POINT ( 'NONE',  ( 75.00000000000000000, -54.99999999999999289, 27.50000000000000000 ) ) ;
#7548 = CYLINDRICAL_SURFACE ( 'NONE', #8206, 5.499999999999991118 ) ;
#7549 = AXIS2_PLACEMENT_3D ( 'NONE', #4932, #981, #2949 ) ;
#7550 = VECTOR ( 'NONE', #5357, 1000.000000000000000 ) ;
#7551 = FACE_BOUND ( 'NONE', #6770, .T. ) ;
#7552 = EDGE_CURVE ( 'NONE', #1049, #1281, #6869, .T. ) ;
#7553 = VECTOR ( 'NONE', #8029, 999.9999999999998863 ) ;
#7554 = VECTOR ( 'NONE', #2662, 1000.000000000000000 ) ;
#7555 = VERTEX_POINT ( 'NONE', #8116 ) ;
#7556 = LINE ( 'NONE', #1774, #1472 ) ;
#7557 = CARTESIAN_POINT ( 'NONE',  ( 115.0000000000000284, -115.0000000000000000, 20.00000000000000355 ) ) ;
#7558 = ORIENTED_EDGE ( 'NONE', *, *, #3954, .F. ) ;
#7559 = DIRECTION ( 'NONE',  ( -0.000000000000000000, -0.000000000000000000, 1.000000000000000000 ) ) ;
#7560 = CARTESIAN_POINT ( 'NONE',  ( 115.0000000000000284, -115.0000000000000000, 70.00000000000000000 ) ) ;
#7561 = CONTEXT_DEPENDENT_SHAPE_REPRESENTATION ( #5489, #1161 ) ;
#7562 = AXIS2_PLACEMENT_3D ( 'NONE', #2106, #6598, #821 ) ;
#7563 = CARTESIAN_POINT ( 'NONE',  ( 0.8183949479883679823, 49.99498560413270098, -24.97998898815200164 ) ) ;
#7564 = VERTEX_POINT ( 'NONE', #3580 ) ;
#7565 = CARTESIAN_POINT ( 'NONE',  ( 121.0000000000000000, 115.0000000000000000, 70.00000000000000000 ) ) ;
#7566 = ORIENTED_EDGE ( 'NONE', *, *, #5207, .T. ) ;
#7567 = CARTESIAN_POINT ( 'NONE',  ( 0.000000000000000000, 0.000000000000000000, 35.00000000000000000 ) ) ;
#7568 = VERTEX_POINT ( 'NONE', #7453 ) ;
#7569 = CARTESIAN_POINT ( 'NONE',  ( 14.30908802125418511, 4.500000000000000000, -120.5000000000000284 ) ) ;
#7570 = DIRECTION ( 'NONE',  ( 1.000000000000000000, 0.000000000000000000, 0.000000000000000000 ) ) ;
#7571 = ORIENTED_EDGE ( 'NONE', *, *, #2734, .F. ) ;
#7572 = CARTESIAN_POINT ( 'NONE',  ( -55.00000000000000711, 55.00000000000000000, 216.9956969048622284 ) ) ;
#7573 = ORIENTED_EDGE ( 'NONE', *, *, #1938, .F. ) ;
#7574 = ORIENTED_EDGE ( 'NONE', *, *, #4058, .T. ) ;
#7575 = DIRECTION ( 'NONE',  ( -0.000000000000000000, -1.632680918566406547E-16, -1.000000000000000000 ) ) ;
#7576 = PRODUCT_DEFINITION ( 'UNKNOWN', '', #3260, #2532 ) ;
#7577 = DIRECTION ( 'NONE',  ( -0.000000000000000000, -1.000000000000000000, 1.586032892321652236E-16 ) ) ;
#7578 = EDGE_CURVE ( 'NONE', #3120, #2214, #6682, .T. ) ;
#7579 = VERTEX_POINT ( 'NONE', #4772 ) ;
#7580 = CARTESIAN_POINT ( 'NONE',  ( -125.0000000000000000, -120.0000000000000000, 0.000000000000000000 ) ) ;
#7581 = EDGE_CURVE ( 'NONE', #2291, #3867, #4901, .T. ) ;
#7582 = AXIS2_PLACEMENT_3D ( 'NONE', #4630, #146, #7212 ) ;
#7583 = SHAPE_REPRESENTATION_RELATIONSHIP ( 'NONE' , 'NONE' ,  #239, #5528 ) ;
#7584 = SURFACE_STYLE_USAGE ( .BOTH. , #6899 ) ;
#7585 = VERTEX_POINT ( 'NONE', #6043 ) ;
#7586 = LINE ( 'NONE', #2443, #6014 ) ;
#7587 = DIRECTION ( 'NONE',  ( -0.000000000000000000, -0.000000000000000000, -1.000000000000000000 ) ) ;
#7588 = DIRECTION ( 'NONE',  ( -0.000000000000000000, 0.000000000000000000, 1.000000000000000000 ) ) ;
#7589 = CARTESIAN_POINT ( 'NONE',  ( -99.49999999999998579, 0.000000000000000000, 12.50000000000000000 ) ) ;
#7590 = EDGE_CURVE ( 'NONE', #3183, #4967, #4838, .T. ) ;
#7591 = CYLINDRICAL_SURFACE ( 'NONE', #652, 5.999999999999991118 ) ;
#7592 = EDGE_LOOP ( 'NONE', ( #3793, #884, #3241, #7963 ) ) ;
#7593 = AXIS2_PLACEMENT_3D ( 'NONE', #5243, #3929, #6627 ) ;
#7594 = CYLINDRICAL_SURFACE ( 'NONE', #6296, 15.00000000000000000 ) ;
#7595 = CIRCLE ( 'NONE', #2090, 50.00000000000000000 ) ;
#7596 = EDGE_LOOP ( 'NONE', ( #6655, #82, #6080, #4903 ) ) ;
#7597 = LINE ( 'NONE', #8232, #6858 ) ;
#7598 = DIRECTION ( 'NONE',  ( 0.000000000000000000, -0.5000000000000011102, -0.8660254037844379305 ) ) ;
#7599 = ORIENTED_EDGE ( 'NONE', *, *, #5261, .T. ) ;
#7600 = AXIS2_PLACEMENT_3D ( 'NONE', #7230, #5878, #6065 ) ;
#7601 = CARTESIAN_POINT ( 'NONE',  ( 10.00000000000000000, -55.00000000000000711, 93.74999999999998579 ) ) ;
#7602 = EDGE_CURVE ( 'NONE', #805, #326, #5922, .T. ) ;
#7603 = LINE ( 'NONE', #3446, #1222 ) ;
#7604 = APPLICATION_PROTOCOL_DEFINITION ( 'draft international standard', 'automotive_design', 1998, #2481 ) ;
#7605 = ORIENTED_EDGE ( 'NONE', *, *, #5537, .T. ) ;
#7606 = CARTESIAN_POINT ( 'NONE',  ( 5.541544814107237649, 49.69330507166041144, -23.71206720076230923 ) ) ;
#7607 = CARTESIAN_POINT ( 'NONE',  ( 10.00000000000000000, -3.448762466456902719E-14, 151.7499999999999432 ) ) ;
#7608 = EDGE_CURVE ( 'NONE', #7187, #2048, #703, .T. ) ;
#7609 = ORIENTED_EDGE ( 'NONE', *, *, #1486, .T. ) ;
#7610 = DIRECTION ( 'NONE',  ( -0.000000000000000000, 0.000000000000000000, 1.000000000000000000 ) ) ;
#7611 = ORIENTED_EDGE ( 'NONE', *, *, #3991, .F. ) ;
#7612 = AXIS2_PLACEMENT_3D ( 'NONE', #6893, #6630, #7270 ) ;
#7613 = DIRECTION ( 'NONE',  ( 1.000000000000000000, 0.000000000000000000, 0.000000000000000000 ) ) ;
#7614 = CARTESIAN_POINT ( 'NONE',  ( -12.33692650994067463, 48.45417487488279562, -14.55343858072927432 ) ) ;
#7615 = ORIENTED_EDGE ( 'NONE', *, *, #3533, .F. ) ;
#7616 = VECTOR ( 'NONE', #5277, 1000.000000000000000 ) ;
#7617 = EDGE_LOOP ( 'NONE', ( #739, #7303, #4373, #6084 ) ) ;
#7618 = CARTESIAN_POINT ( 'NONE',  ( -108.9999999999999147, 115.0000000000000000, 8.205133554287239938E-16 ) ) ;
#7619 = DIRECTION ( 'NONE',  ( 0.000000000000000000, 0.000000000000000000, -1.000000000000000000 ) ) ;
#7620 = LINE ( 'NONE', #4991, #8229 ) ;
#7621 = EDGE_LOOP ( 'NONE', ( #5478, #6921, #5591, #4369 ) ) ;
#7622 = FILL_AREA_STYLE ('',( #5031 ) ) ;
#7623 = DIRECTION ( 'NONE',  ( 1.023826650832276462E-29, 1.033438071402920988E-30, 0.9999999999999998890 ) ) ;
#7624 = PRESENTATION_STYLE_ASSIGNMENT (( #7584 ) ) ;
#7625 = EDGE_LOOP ( 'NONE', ( #5864, #2558, #6432, #3368 ) ) ;
#7626 = EDGE_CURVE ( 'NONE', #7256, #5497, #257, .T. ) ;
#7627 = DIRECTION ( 'NONE',  ( -0.000000000000000000, -0.000000000000000000, 1.000000000000000000 ) ) ;
#7628 = FACE_BOUND ( 'NONE', #3190, .T. ) ;
#7629 = FACE_OUTER_BOUND ( 'NONE', #4275, .T. ) ;
#7630 = CARTESIAN_POINT ( 'NONE',  ( 0.000000000000000000, -125.0000000000000568, 79.99999999999997158 ) ) ;
#7631 = CARTESIAN_POINT ( 'NONE',  ( 6.274835263354066939, -49.60946935866542162, -1.658027691731849496 ) ) ;
#7632 = LINE ( 'NONE', #4441, #1569 ) ;
#7633 = LINE ( 'NONE', #6992, #3995 ) ;
#7634 = EDGE_LOOP ( 'NONE', ( #6118, #8112, #2647, #1641 ) ) ;
#7635 = EDGE_CURVE ( 'NONE', #2500, #836, #3348, .T. ) ;
#7636 = EDGE_CURVE ( 'NONE', #3982, #4695, #5630, .T. ) ;
#7637 = ORIENTED_EDGE ( 'NONE', *, *, #5354, .F. ) ;
#7638 = CARTESIAN_POINT ( 'NONE',  ( -115.0000000000000000, 115.0000000000000000, 20.00000000000000355 ) ) ;
#7639 = ADVANCED_BREP_SHAPE_REPRESENTATION ( '', ( #6411, #1299 ), #6550 ) ;
#7640 = AXIS2_PLACEMENT_3D ( 'NONE', #54, #3259, #6314 ) ;
#7641 = ORIENTED_EDGE ( 'NONE', *, *, #286, .T. ) ;
#7642 = LINE ( 'NONE', #1860, #7132 ) ;
#7643 = AXIS2_PLACEMENT_3D ( 'NONE', #7959, #7286, #1505 ) ;
#7644 = CARTESIAN_POINT ( 'NONE',  ( 125.0000000000000000, 125.0000000000000284, 70.00000000000000000 ) ) ;
#7645 = CIRCLE ( 'NONE', #338, 75.00000000000001421 ) ;
#7646 = ORIENTED_EDGE ( 'NONE', *, *, #4024, .T. ) ;
#7647 = CONTEXT_DEPENDENT_SHAPE_REPRESENTATION ( #3637, #2450 ) ;
#7648 = AXIS2_PLACEMENT_3D ( 'NONE', #4503, #2508, #7018 ) ;
#7649 = ORIENTED_EDGE ( 'NONE', *, *, #7484, .F. ) ;
#7650 = CARTESIAN_POINT ( 'NONE',  ( 11.38780311525837696, 48.68618002971793146, -17.67075055658902372 ) ) ;
#7651 = VECTOR ( 'NONE', #4606, 1000.000000000000000 ) ;
#7652 = EDGE_CURVE ( 'NONE', #4172, #6494, #1162, .T. ) ;
#7653 = AXIS2_PLACEMENT_3D ( 'NONE', #6388, #5883, #5300 ) ;
#7654 = ORIENTED_EDGE ( 'NONE', *, *, #581, .T. ) ;
#7655 = LINE ( 'NONE', #6367, #6165 ) ;
#7656 = VERTEX_POINT ( 'NONE', #4385 ) ;
#7657 = AXIS2_PLACEMENT_3D ( 'NONE', #2894, #6147, #4453 ) ;
#7658 = ORIENTED_EDGE ( 'NONE', *, *, #3782, .T. ) ;
#7659 = CARTESIAN_POINT ( 'NONE',  ( -8.557270319823464533, 49.26314968593495536, -3.379276828450693770 ) ) ;
#7660 = DIRECTION ( 'NONE',  ( -1.000000000000000000, 0.000000000000000000, 0.000000000000000000 ) ) ;
#7661 = DIRECTION ( 'NONE',  ( -1.000000000000000000, 0.000000000000000000, -0.000000000000000000 ) ) ;
#7662 = EDGE_CURVE ( 'NONE', #6525, #4158, #4980, .T. ) ;
#7663 = AXIS2_PLACEMENT_3D ( 'NONE', #4736, #3450, #954 ) ;
#7664 = CARTESIAN_POINT ( 'NONE',  ( -114.9999999999999147, 115.0000000000000000, -28.00000000000002487 ) ) ;
#7665 = DIRECTION ( 'NONE',  ( -0.000000000000000000, -1.000000000000000000, -0.000000000000000000 ) ) ;
#7666 = AXIS2_PLACEMENT_3D ( 'NONE', #2251, #6822, #1676 ) ;
#7667 = CARTESIAN_POINT ( 'NONE',  ( 125.0000000000000000, -52.50000000000000000, 190.0000000000000284 ) ) ;
#7668 = PLANE ( 'NONE',  #7143 ) ;
#7669 = ORIENTED_EDGE ( 'NONE', *, *, #6647, .F. ) ;
#7670 = FACE_BOUND ( 'NONE', #3048, .T. ) ;
#7671 =( LENGTH_UNIT ( ) NAMED_UNIT ( * ) SI_UNIT ( .MILLI., .METRE. ) );
#7672 = VECTOR ( 'NONE', #815, 1000.000000000000000 ) ;
#7673 = CIRCLE ( 'NONE', #6162, 5.499999999999991118 ) ;
#7674 = CARTESIAN_POINT ( 'NONE',  ( -125.0000000000000000, -125.0000000000000284, 70.00000000000000000 ) ) ;
#7675 = VECTOR ( 'NONE', #8013, 1000.000000000000000 ) ;
#7676 = CARTESIAN_POINT ( 'NONE',  ( 5.000000000000000000, 2.342598717236902939, -4.057500000000001883 ) ) ;
#7677 = DIRECTION ( 'NONE',  ( 0.000000000000000000, 0.000000000000000000, -1.000000000000000000 ) ) ;
#7678 = AXIS2_PLACEMENT_3D ( 'NONE', #1607, #1052, #974 ) ;
#7679 = VECTOR ( 'NONE', #7166, 1000.000000000000000 ) ;
#7680 = DIRECTION ( 'NONE',  ( 1.000000000000000000, 0.000000000000000000, 0.000000000000000000 ) ) ;
#7681 = EDGE_LOOP ( 'NONE', ( #2281, #3753, #7357, #1520 ) ) ;
#7682 = CARTESIAN_POINT ( 'NONE',  ( -55.00000000000000000, 55.00000000000000000, 220.0000000000000284 ) ) ;
#7683 = ORIENTED_EDGE ( 'NONE', *, *, #3809, .T. ) ;
#7684 = EDGE_LOOP ( 'NONE', ( #2943, #7863, #4566, #5758 ) ) ;
#7685 = CARTESIAN_POINT ( 'NONE',  ( -125.0000000000000000, -125.0000000000000284, 70.00000000000000000 ) ) ;
#7686 = EDGE_CURVE ( 'NONE', #431, #4314, #520, .T. ) ;
#7687 = AXIS2_PLACEMENT_3D ( 'NONE', #1716, #439, #8004 ) ;
#7688 = CIRCLE ( 'NONE', #1475, 12.99999999999999822 ) ;
#7689 = ORIENTED_EDGE ( 'NONE', *, *, #6123, .F. ) ;
#7690 = DIRECTION ( 'NONE',  ( -0.000000000000000000, -0.000000000000000000, 1.000000000000000000 ) ) ;
#7691 = CARTESIAN_POINT ( 'NONE',  ( -114.9999999999999858, -114.9999999999999858, 20.00000000000000000 ) ) ;
#7692 = ADVANCED_FACE ( 'NONE', ( #4473 ), #1119, .F. ) ;
#7693 = ITEM_DEFINED_TRANSFORMATION ( 'NONE', 'NONE', #6506,  #1299 ) ;
#7694 = ADVANCED_FACE ( 'NONE', ( #8294 ), #3093, .F. ) ;
#7695 = ORIENTED_EDGE ( 'NONE', *, *, #8128, .F. ) ;
#7696 = CARTESIAN_POINT ( 'NONE',  ( 2.050159205374804561, 49.95957628852642074, -24.83755891087361078 ) ) ;
#7697 = AXIS2_PLACEMENT_3D ( 'NONE', #3959, #3436, #5318 ) ;
#7698 = EDGE_LOOP ( 'NONE', ( #2253, #3330, #6179 ) ) ;
#7699 = DIRECTION ( 'NONE',  ( 0.000000000000000000, 0.000000000000000000, 1.000000000000000000 ) ) ;
#7700 = EDGE_LOOP ( 'NONE', ( #4937, #1737, #7227, #7503 ) ) ;
#7701 = CYLINDRICAL_SURFACE ( 'NONE', #2440, 5.999999999999991118 ) ;
#7702 = AXIS2_PLACEMENT_3D ( 'NONE', #7186, #5292, #774 ) ;
#7703 = ADVANCED_FACE ( 'NONE', ( #477 ), #8165, .F. ) ;
#7704 = EDGE_CURVE ( 'NONE', #4085, #5395, #1753, .T. ) ;
#7705 = CARTESIAN_POINT ( 'NONE',  ( 0.000000000000000000, 0.000000000000000000, 0.000000000000000000 ) ) ;
#7706 = VECTOR ( 'NONE', #1014, 1000.000000000000000 ) ;
#7707 = CARTESIAN_POINT ( 'NONE',  ( -6.614448519079573430, 49.56174273647123130, -23.11440585317445695 ) ) ;
#7708 = CARTESIAN_POINT ( 'NONE',  ( 125.0000000000000000, 52.49999999999997158, 0.000000000000000000 ) ) ;
#7709 = ORIENTED_EDGE ( 'NONE', *, *, #7552, .F. ) ;
#7710 = DIRECTION ( 'NONE',  ( -0.000000000000000000, -0.000000000000000000, 1.000000000000000000 ) ) ;
#7711 = CARTESIAN_POINT ( 'NONE',  ( 95.00000000000008527, 0.000000000000000000, 20.00000000000000355 ) ) ;
#7712 = VECTOR ( 'NONE', #977, 1000.000000000000000 ) ;
#7713 = PRODUCT_DEFINITION_SHAPE ( 'NONE', 'NONE',  #8349 ) ;
#7714 = FACE_BOUND ( 'NONE', #466, .T. ) ;
#7715 = EDGE_LOOP ( 'NONE', ( #1342, #3770, #524 ) ) ;
#7716 = EDGE_CURVE ( 'NONE', #5533, #4717, #4341, .T. ) ;
#7717 = CARTESIAN_POINT ( 'NONE',  ( -6.266608689623121897, -49.60708521373747715, -23.32352924753793033 ) ) ;
#7718 = ADVANCED_FACE ( 'NONE', ( #7061, #3847 ), #7668, .T. ) ;
#7719 =( NAMED_UNIT ( * ) PLANE_ANGLE_UNIT ( ) SI_UNIT ( $, .RADIAN. ) );
#7720 =( REPRESENTATION_RELATIONSHIP ('NONE','NONE', #6882, #239 ) REPRESENTATION_RELATIONSHIP_WITH_TRANSFORMATION ( #7335 )SHAPE_REPRESENTATION_RELATIONSHIP( ) );
#7721 = EDGE_LOOP ( 'NONE', ( #6454, #2547, #3519, #1768 ) ) ;
#7722 = EDGE_LOOP ( 'NONE', ( #4498, #2024, #6976, #2983 ) ) ;
#7723 = CARTESIAN_POINT ( 'NONE',  ( -54.99999999999999289, -55.00000000000000711, -27.50000000000000000 ) ) ;
#7724 = VECTOR ( 'NONE', #6620, 1000.000000000000000 ) ;
#7725 = DIRECTION ( 'NONE',  ( 0.000000000000000000, -1.000000000000000000, 0.000000000000000000 ) ) ;
#7726 = CARTESIAN_POINT ( 'NONE',  ( 7.627277604625000151, -49.41585025822053723, -2.588352797709359887 ) ) ;
#7727 = LINE ( 'NONE', #4482, #6270 ) ;
#7728 = FACE_OUTER_BOUND ( 'NONE', #3866, .T. ) ;
#7729 = CARTESIAN_POINT ( 'NONE',  ( 109.5000000000000142, -114.9999999999999716, 20.00000000000000000 ) ) ;
#7730 = ORIENTED_EDGE ( 'NONE', *, *, #4881, .T. ) ;
#7731 = ORIENTED_EDGE ( 'NONE', *, *, #295, .F. ) ;
#7732 = EDGE_LOOP ( 'NONE', ( #4970, #3686, #4735, #332 ) ) ;
#7733 = CARTESIAN_POINT ( 'NONE',  ( 99.49999999999998579, 1.530808498934191521E-15, -12.50000000000000000 ) ) ;
#7734 = ORIENTED_EDGE ( 'NONE', *, *, #5828, .F. ) ;
#7735 = DIRECTION ( 'NONE',  ( -0.000000000000000000, -0.000000000000000000, -1.000000000000000000 ) ) ;
#7736 = CIRCLE ( 'NONE', #3380, 75.00000000000001421 ) ;
#7737 = DIRECTION ( 'NONE',  ( 0.000000000000000000, 1.000000000000000000, 0.000000000000000000 ) ) ;
#7738 = DIRECTION ( 'NONE',  ( 1.000000000000000000, 0.000000000000000000, 0.000000000000000000 ) ) ;
#7739 = LINE ( 'NONE', #6402, #7300 ) ;
#7740 = ORIENTED_EDGE ( 'NONE', *, *, #51, .F. ) ;
#7741 = VECTOR ( 'NONE', #6593, 1000.000000000000000 ) ;
#7742 = AXIS2_PLACEMENT_3D ( 'NONE', #1210, #6983, #4510 ) ;
#7743 = EDGE_CURVE ( 'NONE', #2048, #6246, #3097, .T. ) ;
#7744 = FACE_OUTER_BOUND ( 'NONE', #6168, .T. ) ;
#7745 = EDGE_CURVE ( 'NONE', #5855, #6775, #7620, .T. ) ;
#7746 = ORIENTED_EDGE ( 'NONE', *, *, #3375, .F. ) ;
#7747 = DIRECTION ( 'NONE',  ( 0.000000000000000000, 1.632680918566406547E-16, 1.000000000000000000 ) ) ;
#7748 = FACE_OUTER_BOUND ( 'NONE', #1386, .T. ) ;
#7749 = CARTESIAN_POINT ( 'NONE',  ( 55.00000000000000711, -75.00000000000000000, 27.50000000000000000 ) ) ;
#7750 = EDGE_LOOP ( 'NONE', ( #3897, #4853, #2039, #1307 ) ) ;
#7751 = EDGE_CURVE ( 'NONE', #549, #8146, #3724, .T. ) ;
#7752 = ADVANCED_FACE ( 'NONE', ( #5075, #2999 ), #5029, .F. ) ;
#7753 = DIRECTION ( 'NONE',  ( 0.000000000000000000, 1.000000000000000000, 0.000000000000000000 ) ) ;
#7754 = DIRECTION ( 'NONE',  ( 0.7071067811865474617, 0.000000000000000000, -0.7071067811865474617 ) ) ;
#7755 = ORIENTED_EDGE ( 'NONE', *, *, #5944, .F. ) ;
#7756 = CARTESIAN_POINT ( 'NONE',  ( 125.0000000000000000, 52.49999999999997158, 0.000000000000000000 ) ) ;
#7757 = DIRECTION ( 'NONE',  ( -0.9873608237139801513, 4.107969146635961368E-16, 0.1584884973581719425 ) ) ;
#7758 = CIRCLE ( 'NONE', #5446, 4.999999999999990230 ) ;
#7759 = ORIENTED_EDGE ( 'NONE', *, *, #6765, .T. ) ;
#7760 = EDGE_LOOP ( 'NONE', ( #6686, #4400 ) ) ;
#7761 = DIRECTION ( 'NONE',  ( -1.000000000000000000, 0.000000000000000000, 0.000000000000000000 ) ) ;
#7762 = AXIS2_PLACEMENT_3D ( 'NONE', #1516, #5979, #6095 ) ;
#7763 = DIRECTION ( 'NONE',  ( -1.000000000000000000, -0.000000000000000000, -0.000000000000000000 ) ) ;
#7764 = CARTESIAN_POINT ( 'NONE',  ( 4.429756409623588631, -49.80481938051303814, -0.8041353051610896641 ) ) ;
#7765 = DIRECTION ( 'NONE',  ( 1.000000000000000000, 0.000000000000000000, 0.000000000000000000 ) ) ;
#7766 =( NAMED_UNIT ( * ) PLANE_ANGLE_UNIT ( ) SI_UNIT ( $, .RADIAN. ) );
#7767 = PRESENTATION_LAYER_ASSIGNMENT (  '', '', ( #5733 ) ) ;
#7768 = CARTESIAN_POINT ( 'NONE',  ( -125.0000000000000000, 125.0000000000000000, 20.00000000000000000 ) ) ;
#7769 = ORIENTED_EDGE ( 'NONE', *, *, #6371, .T. ) ;
#7770 = ADVANCED_FACE ( 'NONE', ( #3774 ), #4429, .T. ) ;
#7771 = ORIENTED_EDGE ( 'NONE', *, *, #1024, .F. ) ;
#7772 = ORIENTED_EDGE ( 'NONE', *, *, #5940, .T. ) ;
#7773 = CARTESIAN_POINT ( 'NONE',  ( -121.0000000000000000, 115.0000000000000000, 20.00000000000000355 ) ) ;
#7774 = EDGE_LOOP ( 'NONE', ( #3562, #6624, #580, #427 ) ) ;
#7775 = DIRECTION ( 'NONE',  ( 1.000000000000000000, 0.000000000000000000, 0.000000000000000000 ) ) ;
#7776 = CARTESIAN_POINT ( 'NONE',  ( -54.99999999999999289, -55.00000000000000711, 27.50000000000000000 ) ) ;
#7777 = DIRECTION ( 'NONE',  ( 1.000000000000000000, 0.000000000000000000, 0.000000000000000000 ) ) ;
#7778 = CONTEXT_DEPENDENT_SHAPE_REPRESENTATION ( #6393, #1986 ) ;
#7779 = DIRECTION ( 'NONE',  ( -0.000000000000000000, -0.000000000000000000, -1.000000000000000000 ) ) ;
#7780 = PRODUCT_DEFINITION_SHAPE ( 'NONE', 'NONE',  #8371 ) ;
#7781 = CIRCLE ( 'NONE', #6133, 75.00000000000001421 ) ;
#7782 = PLANE ( 'NONE',  #3757 ) ;
#7783 = ORIENTED_EDGE ( 'NONE', *, *, #8093, .F. ) ;
#7784 = VECTOR ( 'NONE', #5127, 1000.000000000000000 ) ;
#7785 = CARTESIAN_POINT ( 'NONE',  ( 0.000000000000000000, 0.000000000000000000, -120.5000000000000284 ) ) ;
#7786 = ADVANCED_FACE ( 'NONE', ( #5117, #7714 ), #1931, .T. ) ;
#7787 = CARTESIAN_POINT ( 'NONE',  ( -25.00000000000000000, 0.000000000000000000, -120.5000000000000284 ) ) ;
#7788 = CARTESIAN_POINT ( 'NONE',  ( -124.0000000000000000, -114.9999999999999858, 10.00000000000000000 ) ) ;
#7789 = LINE ( 'NONE', #7836, #854 ) ;
#7790 = CIRCLE ( 'NONE', #4118, 5.000000000000004441 ) ;
#7791 = DIRECTION ( 'NONE',  ( 0.000000000000000000, 0.000000000000000000, 1.000000000000000000 ) ) ;
#7792 = CARTESIAN_POINT ( 'NONE',  ( 125.0000000000000000, -125.0000000000000000, -28.00000000000002487 ) ) ;
#7793 = DIRECTION ( 'NONE',  ( -1.000000000000000000, 0.000000000000000000, 0.000000000000000000 ) ) ;
#7794 = ORIENTED_EDGE ( 'NONE', *, *, #5323, .T. ) ;
#7795 = DIRECTION ( 'NONE',  ( 0.000000000000000000, 0.000000000000000000, -1.000000000000000000 ) ) ;
#7796 = DIRECTION ( 'NONE',  ( 1.000000000000000000, 0.000000000000000000, 0.000000000000000000 ) ) ;
#7797 = EDGE_CURVE ( 'NONE', #4180, #7487, #1451, .T. ) ;
#7798 = EDGE_CURVE ( 'NONE', #6076, #1436, #534, .T. ) ;
#7799 = EDGE_LOOP ( 'NONE', ( #1228, #5677, #7535, #6075 ) ) ;
#7800 = VECTOR ( 'NONE', #4504, 1000.000000000000000 ) ;
#7801 = VECTOR ( 'NONE', #704, 1000.000000000000000 ) ;
#7802 = DIRECTION ( 'NONE',  ( -0.000000000000000000, -0.000000000000000000, -1.000000000000000000 ) ) ;
#7803 = DIRECTION ( 'NONE',  ( -0.000000000000000000, -0.000000000000000000, 1.000000000000000000 ) ) ;
#7804 = DIRECTION ( 'NONE',  ( -1.000000000000000000, 0.000000000000000000, 0.000000000000000000 ) ) ;
#7805 = DIRECTION ( 'NONE',  ( -0.000000000000000000, -0.000000000000000000, 1.000000000000000000 ) ) ;
#7806 = EDGE_CURVE ( 'NONE', #3864, #1662, #1620, .T. ) ;
#7807 = EDGE_CURVE ( 'NONE', #448, #5909, #816, .T. ) ;
#7808 = FACE_OUTER_BOUND ( 'NONE', #1874, .T. ) ;
#7809 = VERTEX_POINT ( 'NONE', #7145 ) ;
#7810 = AXIS2_PLACEMENT_3D ( 'NONE', #370, #2947, #1612 ) ;
#7811 = CARTESIAN_POINT ( 'NONE',  ( -10.00000000000000000, -3.448762466456902719E-14, 93.74999999999998579 ) ) ;
#7812 = ORIENTED_EDGE ( 'NONE', *, *, #308, .F. ) ;
#7813 = AXIS2_PLACEMENT_3D ( 'NONE', #4587, #3714, #5857 ) ;
#7814 = ORIENTED_EDGE ( 'NONE', *, *, #5314, .T. ) ;
#7815 = FACE_OUTER_BOUND ( 'NONE', #4221, .T. ) ;
#7816 = ORIENTED_EDGE ( 'NONE', *, *, #3763, .T. ) ;
#7817 = DIRECTION ( 'NONE',  ( 0.000000000000000000, 1.000000000000000000, -1.266875999117951024E-16 ) ) ;
#7818 = FACE_OUTER_BOUND ( 'NONE', #4558, .T. ) ;
#7819 = VECTOR ( 'NONE', #235, 1000.000000000000000 ) ;
#7820 = ORIENTED_EDGE ( 'NONE', *, *, #4720, .F. ) ;
#7821 = EDGE_CURVE ( 'NONE', #321, #4413, #4, .T. ) ;
#7822 = EDGE_CURVE ( 'NONE', #2601, #3678, #5532, .T. ) ;
#7823 = CARTESIAN_POINT ( 'NONE',  ( 75.00000000000000000, -75.00000000000000000, -27.50000000000000000 ) ) ;
#7824 = EDGE_LOOP ( 'NONE', ( #3567, #405, #631, #7816 ) ) ;
#7825 = AXIS2_PLACEMENT_3D ( 'NONE', #5721, #4439, #8303 ) ;
#7826 = AXIS2_PLACEMENT_3D ( 'NONE', #5469, #3593, #6128 ) ;
#7827 = DIRECTION ( 'NONE',  ( 0.000000000000000000, 0.000000000000000000, 1.000000000000000000 ) ) ;
#7828 = VERTEX_POINT ( 'NONE', #7226 ) ;
#7829 = DIRECTION ( 'NONE',  ( 0.8571673007021116675, 0.000000000000000000, 0.5150380749100552658 ) ) ;
#7830 = VECTOR ( 'NONE', #7102, 1000.000000000000000 ) ;
#7831 = CIRCLE ( 'NONE', #4155, 5.999999999999991118 ) ;
#7832 = FACE_OUTER_BOUND ( 'NONE', #7045, .T. ) ;
#7833 = CARTESIAN_POINT ( 'NONE',  ( 0.000000000000000000, 0.000000000000000000, 0.000000000000000000 ) ) ;
#7834 = LINE ( 'NONE', #3398, #7930 ) ;
#7835 = AXIS2_PLACEMENT_3D ( 'NONE', #5589, #43, #4647 ) ;
#7836 = CARTESIAN_POINT ( 'NONE',  ( -1.378709915621162062E-13, -12.50000000000001243, -54.99999999999995026 ) ) ;
#7837 = DIRECTION ( 'NONE',  ( 1.000000000000000000, 0.000000000000000000, 0.000000000000000000 ) ) ;
#7838 = CARTESIAN_POINT ( 'NONE',  ( 125.0000000000000000, 125.0000000000000284, 0.000000000000000000 ) ) ;
#7839 = EDGE_LOOP ( 'NONE', ( #7431, #6292 ) ) ;
#7840 = CARTESIAN_POINT ( 'NONE',  ( -125.0000000000000000, -120.0000000000000000, -28.00000000000002487 ) ) ;
#7841 = DIRECTION ( 'NONE',  ( 0.000000000000000000, 0.000000000000000000, -1.000000000000000000 ) ) ;
#7842 = ORIENTED_EDGE ( 'NONE', *, *, #3279, .T. ) ;
#7843 = CARTESIAN_POINT ( 'NONE',  ( 14.30908802125418511, -4.500000000000000000, -28.00000000000002487 ) ) ;
#7844 = EDGE_CURVE ( 'NONE', #4855, #6775, #2065, .T. ) ;
#7845 = CARTESIAN_POINT ( 'NONE',  ( -121.0000000000000000, 115.0000000000000000, 70.00000000000000000 ) ) ;
#7846 = FACE_BOUND ( 'NONE', #5222, .T. ) ;
#7847 = DIRECTION ( 'NONE',  ( -0.000000000000000000, -0.000000000000000000, 1.000000000000000000 ) ) ;
#7848 = PRODUCT_DEFINITION_SHAPE ( 'NONE', 'NONE',  #8356 ) ;
#7849 = CARTESIAN_POINT ( 'NONE',  ( 120.9999999999999005, -115.0000000000000000, 0.000000000000000000 ) ) ;
#7850 = ORIENTED_EDGE ( 'NONE', *, *, #6788, .F. ) ;
#7851 = EDGE_CURVE ( 'NONE', #3745, #4528, #2595, .T. ) ;
#7852 = EDGE_LOOP ( 'NONE', ( #7141, #3834 ) ) ;
#7853 = CARTESIAN_POINT ( 'NONE',  ( -75.00000000000001421, 0.000000000000000000, 15.00000000000000000 ) ) ;
#7854 = EDGE_CURVE ( 'NONE', #6896, #3808, #4557, .T. ) ;
#7855 = ORIENTED_EDGE ( 'NONE', *, *, #6560, .F. ) ;
#7856 = FACE_OUTER_BOUND ( 'NONE', #6981, .T. ) ;
#7857 = CARTESIAN_POINT ( 'NONE',  ( 10.40000000000000036, 0.000000000000000000, 0.000000000000000000 ) ) ;
#7858 = ADVANCED_BREP_SHAPE_REPRESENTATION ( '', ( #3442, #1299 ), #4925 ) ;
#7859 = CARTESIAN_POINT ( 'NONE',  ( -110.0000000000000142, -115.0000000000000000, 270.0000000000000000 ) ) ;
#7860 = VERTEX_POINT ( 'NONE', #166 ) ;
#7861 = LINE ( 'NONE', #1960, #7616 ) ;
#7862 = CARTESIAN_POINT ( 'NONE',  ( 124.0000000000000000, -114.9999999999999716, 20.00000000000000000 ) ) ;
#7863 = ORIENTED_EDGE ( 'NONE', *, *, #1851, .T. ) ;
#7864 = DIRECTION ( 'NONE',  ( 0.8571673007021116675, 0.000000000000000000, 0.5150380749100552658 ) ) ;
#7865 = VECTOR ( 'NONE', #8330, 1000.000000000000000 ) ;
#7866 = DIRECTION ( 'NONE',  ( -0.000000000000000000, -7.945337353457666666E-18, -1.000000000000000000 ) ) ;
#7867 = APPLICATION_CONTEXT ( 'automotive_design' ) ;
#7868 = LINE ( 'NONE', #2631, #5319 ) ;
#7869 = DIRECTION ( 'NONE',  ( -0.8571673007021112234, 1.049727191138617340E-16, 0.5150380749100560429 ) ) ;
#7870 = CARTESIAN_POINT ( 'NONE',  ( -125.0000000000000000, -125.0000000000000000, -28.00000000000002487 ) ) ;
#7871 = CARTESIAN_POINT ( 'NONE',  ( 17.61817604250836311, -4.500000000000000000, -28.00000000000002487 ) ) ;
#7872 = AXIS2_PLACEMENT_3D ( 'NONE', #1690, #4802, #6837 ) ;
#7873 = AXIS2_PLACEMENT_3D ( 'NONE', #3936, #1012, #4650 ) ;
#7874 = CYLINDRICAL_SURFACE ( 'NONE', #7562, 4.999999999999997335 ) ;
#7875 = ORIENTED_EDGE ( 'NONE', *, *, #6975, .T. ) ;
#7876 = FACE_OUTER_BOUND ( 'NONE', #4074, .T. ) ;
#7877 = DIRECTION ( 'NONE',  ( 1.000000000000000000, 3.155443620884047222E-30, 1.224646799147346798E-16 ) ) ;
#7878 = ORIENTED_EDGE ( 'NONE', *, *, #1868, .T. ) ;
#7879 = SPHERICAL_SURFACE ( 'NONE', #222, 3.000000000000001776 ) ;
#7880 = PLANE ( 'NONE',  #2010 ) ;
#7881 = DIRECTION ( 'NONE',  ( 1.000000000000000000, 0.000000000000000000, 0.000000000000000000 ) ) ;
#7882 = DIRECTION ( 'NONE',  ( -1.000000000000000000, -0.000000000000000000, -0.000000000000000000 ) ) ;
#7883 = CONICAL_SURFACE ( 'NONE', #6517, 4.999999999999990230, 1.029744258676656754 ) ;
#7884 = SURFACE_SIDE_STYLE ('',( #2033 ) ) ;
#7885 = CARTESIAN_POINT ( 'NONE',  ( 0.000000000000000000, 125.0000000000000568, 79.99999999999992895 ) ) ;
#7886 = EDGE_CURVE ( 'NONE', #5186, #7159, #4508, .T. ) ;
#7887 = VERTEX_POINT ( 'NONE', #1407 ) ;
#7888 = DIRECTION ( 'NONE',  ( 0.000000000000000000, -7.945337353457666666E-18, -1.000000000000000000 ) ) ;
#7889 = PLANE ( 'NONE',  #1339 ) ;
#7890 = ORIENTED_EDGE ( 'NONE', *, *, #4420, .F. ) ;
#7891 = LINE ( 'NONE', #5938, #6717 ) ;
#7892 = DIRECTION ( 'NONE',  ( 1.000000000000000000, 0.000000000000000000, 0.000000000000000000 ) ) ;
#7893 = VECTOR ( 'NONE', #1292, 1000.000000000000000 ) ;
#7894 = PRODUCT ( 'Upright servo motor', 'Upright servo motor', '', ( #7511 ) ) ;
#7895 = CARTESIAN_POINT ( 'NONE',  ( -125.0000000000000000, 0.000000000000000000, 0.000000000000000000 ) ) ;
#7896 = EDGE_CURVE ( 'NONE', #5876, #6392, #647, .T. ) ;
#7897 = EDGE_CURVE ( 'NONE', #5646, #4085, #6610, .T. ) ;
#7898 = EDGE_CURVE ( 'NONE', #1537, #3078, #540, .T. ) ;
#7899 = ORIENTED_EDGE ( 'NONE', *, *, #921, .F. ) ;
#7900 = ORIENTED_EDGE ( 'NONE', *, *, #460, .T. ) ;
#7901 = CARTESIAN_POINT ( 'NONE',  ( 115.0000000000000000, 114.9999999999999716, 20.00000000000000000 ) ) ;
#7902 = ORIENTED_EDGE ( 'NONE', *, *, #3920, .F. ) ;
#7903 = DIRECTION ( 'NONE',  ( -0.000000000000000000, -0.000000000000000000, 1.000000000000000000 ) ) ;
#7904 = CARTESIAN_POINT ( 'NONE',  ( 0.000000000000000000, 125.0000000000000000, -25.00000000000000000 ) ) ;
#7905 = CARTESIAN_POINT ( 'NONE',  ( -4.429756409623576197, 49.80481938051305235, -0.8041353051610855562 ) ) ;
#7906 = EDGE_CURVE ( 'NONE', #6640, #3678, #6551, .T. ) ;
#7907 = DIRECTION ( 'NONE',  ( 1.000000000000000000, 0.000000000000000000, 0.000000000000000000 ) ) ;
#7908 = PLANE ( 'NONE',  #175 ) ;
#7909 = CARTESIAN_POINT ( 'NONE',  ( -115.0000000000000000, 115.0000000000000000, 340.0000000000000000 ) ) ;
#7910 = AXIS2_PLACEMENT_3D ( 'NONE', #1985, #4521, #7117 ) ;
#7911 = CARTESIAN_POINT ( 'NONE',  ( -75.00000000000000000, -75.00000000000000000, 27.50000000000000000 ) ) ;
#7912 = ORIENTED_EDGE ( 'NONE', *, *, #2616, .F. ) ;
#7913 = DIRECTION ( 'NONE',  ( 0.000000000000000000, -0.5000000000000011102, -0.8660254037844379305 ) ) ;
#7914 = ADVANCED_FACE ( 'NONE', ( #693 ), #3249, .T. ) ;
#7915 = CYLINDRICAL_SURFACE ( 'NONE', #2916, 49.99999999999999289 ) ;
#7916 = CARTESIAN_POINT ( 'NONE',  ( 4.592425496802573578E-15, -37.49999999999999289, -250.0000000000000000 ) ) ;
#7917 = FACE_OUTER_BOUND ( 'NONE', #1341, .T. ) ;
#7918 = DIRECTION ( 'NONE',  ( 1.000000000000000000, 0.000000000000000000, -0.000000000000000000 ) ) ;
#7919 =( NAMED_UNIT ( * ) PLANE_ANGLE_UNIT ( ) SI_UNIT ( $, .RADIAN. ) );
#7920 = VECTOR ( 'NONE', #762, 1000.000000000000000 ) ;
#7921 = CARTESIAN_POINT ( 'NONE',  ( -115.0000000000000000, -115.0000000000000000, 340.0000000000000000 ) ) ;
#7922 = CARTESIAN_POINT ( 'NONE',  ( -55.00000000000000000, -55.00000000000000000, 240.0000000000000284 ) ) ;
#7923 = ORIENTED_EDGE ( 'NONE', *, *, #6854, .F. ) ;
#7924 = CARTESIAN_POINT ( 'NONE',  ( 54.99999999999999289, -55.00000000000000711, 27.50000000000000000 ) ) ;
#7925 = VECTOR ( 'NONE', #7282, 1000.000000000000000 ) ;
#7926 = CARTESIAN_POINT ( 'NONE',  ( 1.592040838891560279E-15, 125.0000000000000568, 92.99999999999992895 ) ) ;
#7927 = CIRCLE ( 'NONE', #6428, 5.400000000000035882 ) ;
#7928 = LINE ( 'NONE', #3916, #6041 ) ;
#7929 = DIRECTION ( 'NONE',  ( 0.000000000000000000, -1.224646799147353207E-16, 1.000000000000000000 ) ) ;
#7930 = VECTOR ( 'NONE', #4602, 1000.000000000000000 ) ;
#7931 = FACE_OUTER_BOUND ( 'NONE', #2081, .T. ) ;
#7932 = AXIS2_PLACEMENT_3D ( 'NONE', #879, #6619, #6574 ) ;
#7933 = VERTEX_POINT ( 'NONE', #5838 ) ;
#7934 = VERTEX_POINT ( 'NONE', #3326 ) ;
#7935 = CYLINDRICAL_SURFACE ( 'NONE', #5504, 12.50000000000000000 ) ;
#7936 = VECTOR ( 'NONE', #2772, 1000.000000000000000 ) ;
#7937 = ORIENTED_EDGE ( 'NONE', *, *, #4381, .F. ) ;
#7938 = ADVANCED_FACE ( 'NONE', ( #123 ), #7874, .F. ) ;
#7939 = CARTESIAN_POINT ( 'NONE',  ( 0.000000000000000000, 50.00000000000000000, 0.000000000000000000 ) ) ;
#7940 = AXIS2_PLACEMENT_3D ( 'NONE', #6783, #5570, #1725 ) ;
#7941 = DIRECTION ( 'NONE',  ( -0.000000000000000000, -0.000000000000000000, 1.000000000000000000 ) ) ;
#7942 = DIRECTION ( 'NONE',  ( 0.000000000000000000, 0.000000000000000000, -1.000000000000000000 ) ) ;
#7943 = PLANE ( 'NONE',  #4899 ) ;
#7944 = EDGE_CURVE ( 'NONE', #836, #66, #5328, .T. ) ;
#7945 = FACE_OUTER_BOUND ( 'NONE', #3843, .T. ) ;
#7946 = EDGE_CURVE ( 'NONE', #758, #2041, #4688, .T. ) ;
#7947 = AXIS2_PLACEMENT_3D ( 'NONE', #7422, #1554, #352 ) ;
#7948 = AXIS2_PLACEMENT_3D ( 'NONE', #853, #121, #3401 ) ;
#7949 = DIRECTION ( 'NONE',  ( -0.000000000000000000, -7.945337353457666666E-18, -1.000000000000000000 ) ) ;
#7950 = ORIENTED_EDGE ( 'NONE', *, *, #31, .F. ) ;
#7951 = CYLINDRICAL_SURFACE ( 'NONE', #1709, 4.999999999999990230 ) ;
#7952 = VERTEX_POINT ( 'NONE', #2369 ) ;
#7953=STYLED_ITEM('',(#8414),#6411);
#7954 = DIRECTION ( 'NONE',  ( 0.000000000000000000, 0.000000000000000000, -1.000000000000000000 ) ) ;
#7955 = ADVANCED_FACE ( 'NONE', ( #1099 ), #4919, .F. ) ;
#7956 = ADVANCED_FACE ( 'NONE', ( #5991 ), #4323, .T. ) ;
#7957 = PRODUCT ( 'Timing belt', 'Timing belt', '', ( #2984 ) ) ;
#7958 = DIRECTION ( 'NONE',  ( 0.000000000000000000, -0.000000000000000000, -1.000000000000000000 ) ) ;
#7959 = CARTESIAN_POINT ( 'NONE',  ( 120.5000000000000000, 114.9999999999999716, 10.00000000000000000 ) ) ;
#7960 = AXIS2_PLACEMENT_3D ( 'NONE', #5875, #5201, #7275 ) ;
#7961 = PLANE ( 'NONE',  #8313 ) ;
#7962 = CARTESIAN_POINT ( 'NONE',  ( 3.061616997868367857E-16, -2.499999999999984013, -246.6833752096445664 ) ) ;
#7963 = ORIENTED_EDGE ( 'NONE', *, *, #2268, .T. ) ;
#7964 = DIRECTION ( 'NONE',  ( 1.000000000000000000, 0.000000000000000000, 0.000000000000000000 ) ) ;
#7965 = FACE_OUTER_BOUND ( 'NONE', #672, .T. ) ;
#7966 = FACE_OUTER_BOUND ( 'NONE', #7732, .T. ) ;
#7967 = VERTEX_POINT ( 'NONE', #7310 ) ;
#7968 = DIRECTION ( 'NONE',  ( -0.000000000000000000, -0.000000000000000000, 1.000000000000000000 ) ) ;
#7969 = CARTESIAN_POINT ( 'NONE',  ( 125.0000000000000000, -52.50000000000000000, 190.0000000000000284 ) ) ;
#7970 = DIRECTION ( 'NONE',  ( 0.000000000000000000, 2.960594732333750117E-16, -1.000000000000000000 ) ) ;
#7971 = CARTESIAN_POINT ( 'NONE',  ( -120.9999999999999005, 115.0000000000000000, 8.205133554287239938E-16 ) ) ;
#7972 = VERTEX_POINT ( 'NONE', #8236 ) ;
#7973 = ORIENTED_EDGE ( 'NONE', *, *, #6113, .F. ) ;
#7974 = CARTESIAN_POINT ( 'NONE',  ( 125.0000000000000000, -125.0000000000000000, -28.00000000000002487 ) ) ;
#7975 = VERTEX_POINT ( 'NONE', #5656 ) ;
#7976 = LINE ( 'NONE', #6703, #7281 ) ;
#7977 = ORIENTED_EDGE ( 'NONE', *, *, #1698, .F. ) ;
#7978 = CARTESIAN_POINT ( 'NONE',  ( 3.243174531372581271, 49.89626761698125534, -0.4210505255250476808 ) ) ;
#7979 = DIRECTION ( 'NONE',  ( -0.000000000000000000, -0.000000000000000000, 1.000000000000000000 ) ) ;
#7980 = EDGE_CURVE ( 'NONE', #7327, #7159, #898, .T. ) ;
#7981 = DIRECTION ( 'NONE',  ( -0.000000000000000000, 1.000000000000000000, -1.266875999117951024E-16 ) ) ;
#7982 = CARTESIAN_POINT ( 'NONE',  ( 0.000000000000000000, 125.0000000000000000, -12.50000000000000000 ) ) ;
#7983 = CARTESIAN_POINT ( 'NONE',  ( 0.000000000000000000, 0.000000000000000000, 35.00000000000000000 ) ) ;
#7984 = DIRECTION ( 'NONE',  ( -1.000000000000000000, -0.000000000000000000, -0.000000000000000000 ) ) ;
#7985 = DIRECTION ( 'NONE',  ( 1.000000000000000000, 0.000000000000000000, 0.000000000000000000 ) ) ;
#7986 = DIRECTION ( 'NONE',  ( 0.000000000000000000, 0.000000000000000000, -1.000000000000000000 ) ) ;
#7987 = AXIS2_PLACEMENT_3D ( 'NONE', #6652, #7888, #791 ) ;
#7988 = VERTEX_POINT ( 'NONE', #6828 ) ;
#7989 = EDGE_CURVE ( 'NONE', #4767, #1268, #3225, .T. ) ;
#7990 = EDGE_CURVE ( 'NONE', #5309, #2019, #411, .T. ) ;
#7991 = ADVANCED_FACE ( 'NONE', ( #6195 ), #455, .F. ) ;
#7992 = EDGE_LOOP ( 'NONE', ( #4113, #3610 ) ) ;
#7993 = FACE_OUTER_BOUND ( 'NONE', #5054, .T. ) ;
#7994 = PRODUCT_DEFINITION_FORMATION_WITH_SPECIFIED_SOURCE ( 'ANY', '', #5056, .NOT_KNOWN. ) ;
#7995 = DIRECTION ( 'NONE',  ( -0.000000000000000000, -0.000000000000000000, -1.000000000000000000 ) ) ;
#7996 = CARTESIAN_POINT ( 'NONE',  ( -12.49965553489658276, -48.41238076809165136, -11.67579978239260541 ) ) ;
#7997 = DIRECTION ( 'NONE',  ( 1.000000000000000000, 0.000000000000000000, 0.000000000000000000 ) ) ;
#7998 = VECTOR ( 'NONE', #876, 1000.000000000000000 ) ;
#7999 = DIRECTION ( 'NONE',  ( -0.000000000000000000, -0.000000000000000000, -1.000000000000000000 ) ) ;
#8000 = VERTEX_POINT ( 'NONE', #4084 ) ;
#8001 = EDGE_CURVE ( 'NONE', #836, #7206, #7603, .T. ) ;
#8002 = DIRECTION ( 'NONE',  ( -0.000000000000000000, -0.000000000000000000, 1.000000000000000000 ) ) ;
#8003 = DIRECTION ( 'NONE',  ( -1.752490724247359037E-17, 1.000000000000000000, 3.853078496550133260E-17 ) ) ;
#8004 = DIRECTION ( 'NONE',  ( 1.000000000000000000, 0.000000000000000000, 0.000000000000000000 ) ) ;
#8005 = DIRECTION ( 'NONE',  ( 0.000000000000000000, 0.000000000000000000, -1.000000000000000000 ) ) ;
#8006 = DIRECTION ( 'NONE',  ( -0.000000000000000000, -0.000000000000000000, 1.000000000000000000 ) ) ;
#8007 = CARTESIAN_POINT ( 'NONE',  ( 115.0000000000000000, -115.0000000000000000, 270.0000000000000000 ) ) ;
#8008 = VECTOR ( 'NONE', #1403, 1000.000000000000000 ) ;
#8009 = EDGE_CURVE ( 'NONE', #4086, #2906, #4766, .T. ) ;
#8010 = ORIENTED_EDGE ( 'NONE', *, *, #1921, .T. ) ;
#8011 = PRODUCT_DEFINITION_CONTEXT ( 'detailed design', #2481, 'design' ) ;
#8012 = ORIENTED_EDGE ( 'NONE', *, *, #7372, .T. ) ;
#8013 = DIRECTION ( 'NONE',  ( 0.000000000000000000, -1.000000000000000000, 0.000000000000000000 ) ) ;
#8014 = ORIENTED_EDGE ( 'NONE', *, *, #5224, .T. ) ;
#8015 = CARTESIAN_POINT ( 'NONE',  ( -50.00000000000000711, 55.00000000000000000, 220.0000000000000284 ) ) ;
#8016 = VECTOR ( 'NONE', #2969, 1000.000000000000000 ) ;
#8017 = APPLICATION_CONTEXT ( 'automotive_design' ) ;
#8018 = ORIENTED_EDGE ( 'NONE', *, *, #1346, .T. ) ;
#8019 = CARTESIAN_POINT ( 'NONE',  ( 95.00000000000002842, -95.00000000000002842, 70.00000000000000000 ) ) ;
#8020 =( GEOMETRIC_REPRESENTATION_CONTEXT ( 3 ) GLOBAL_UNCERTAINTY_ASSIGNED_CONTEXT ( ( #6394 ) ) GLOBAL_UNIT_ASSIGNED_CONTEXT ( ( #1508, #4821, #6121 ) ) REPRESENTATION_CONTEXT ( 'NONE', 'WORKASPACE' ) );
#8021 = CARTESIAN_POINT ( 'NONE',  ( 17.61817604250836311, -4.500000000000000000, -128.0000000000000284 ) ) ;
#8022 = LINE ( 'NONE', #3443, #1412 ) ;
#8023 = DIRECTION ( 'NONE',  ( 0.000000000000000000, -1.266875999117951024E-16, 1.000000000000000000 ) ) ;
#8024 = DIRECTION ( 'NONE',  ( 0.000000000000000000, 0.000000000000000000, 1.000000000000000000 ) ) ;
#8025 = VERTEX_POINT ( 'NONE', #1053 ) ;
#8026 = VERTEX_POINT ( 'NONE', #2413 ) ;
#8027 = ORIENTED_EDGE ( 'NONE', *, *, #4633, .F. ) ;
#8028 = DIRECTION ( 'NONE',  ( -1.000000000000000000, 0.000000000000000000, -0.000000000000000000 ) ) ;
#8029 = DIRECTION ( 'NONE',  ( -0.7071067811865420216, 8.659560562355001884E-17, -0.7071067811865531239 ) ) ;
#8030 = ADVANCED_FACE ( 'NONE', ( #7356 ), #6031, .F. ) ;
#8031 = ADVANCED_FACE ( 'NONE', ( #3067 ), #5365, .F. ) ;
#8032 = ORIENTED_EDGE ( 'NONE', *, *, #3961, .F. ) ;
#8033 =( NAMED_UNIT ( * ) PLANE_ANGLE_UNIT ( ) SI_UNIT ( $, .RADIAN. ) );
#8034 = PRESENTATION_STYLE_ASSIGNMENT (( #6728 ) ) ;
#8035 = DIRECTION ( 'NONE',  ( 0.000000000000000000, 0.000000000000000000, 1.000000000000000000 ) ) ;
#8036 = EDGE_LOOP ( 'NONE', ( #6974, #2613, #2209, #2119 ) ) ;
#8037 = AXIS2_PLACEMENT_3D ( 'NONE', #5600, #7423, #4184 ) ;
#8038 = CYLINDRICAL_SURFACE ( 'NONE', #6498, 5.999999999999991118 ) ;
#8039 = CYLINDRICAL_SURFACE ( 'NONE', #2297, 4.999999999999990230 ) ;
#8040 = CIRCLE ( 'NONE', #2007, 5.499999999999991118 ) ;
#8041 = EDGE_LOOP ( 'NONE', ( #3254, #5806, #3201, #4529 ) ) ;
#8042 = CARTESIAN_POINT ( 'NONE',  ( 121.0000000000000000, 115.0000000000000000, 70.00000000000000000 ) ) ;
#8043 = EDGE_CURVE ( 'NONE', #4209, #334, #4277, .T. ) ;
#8044 = DIRECTION ( 'NONE',  ( 1.000000000000000000, 0.000000000000000000, 0.000000000000000000 ) ) ;
#8045 = LINE ( 'NONE', #2809, #6391 ) ;
#8046 = DIRECTION ( 'NONE',  ( -0.000000000000000000, -0.000000000000000000, 1.000000000000000000 ) ) ;
#8047 = ORIENTED_EDGE ( 'NONE', *, *, #4501, .F. ) ;
#8048 = VECTOR ( 'NONE', #4394, 1000.000000000000000 ) ;
#8049 = ORIENTED_EDGE ( 'NONE', *, *, #5688, .F. ) ;
#8050 = FACE_OUTER_BOUND ( 'NONE', #6360, .T. ) ;
#8051 = VERTEX_POINT ( 'NONE', #2829 ) ;
#8052 = FACE_OUTER_BOUND ( 'NONE', #6876, .T. ) ;
#8053 = EDGE_CURVE ( 'NONE', #4879, #624, #2982, .T. ) ;
#8054 = DIRECTION ( 'NONE',  ( 0.9992060621654691444, -0.03984024763698791605, 1.223674505719567166E-16 ) ) ;
#8055 = VECTOR ( 'NONE', #5181, 1000.000000000000000 ) ;
#8056 = VERTEX_POINT ( 'NONE', #855 ) ;
#8057 = DIRECTION ( 'NONE',  ( -0.000000000000000000, -0.000000000000000000, 1.000000000000000000 ) ) ;
#8058 = AXIS2_PLACEMENT_3D ( 'NONE', #3957, #2053, #7827 ) ;
#8059 = CARTESIAN_POINT ( 'NONE',  ( -10.00000000000000000, -3.448762466456902719E-14, 151.7499999999999432 ) ) ;
#8060 = LINE ( 'NONE', #4763, #4472 ) ;
#8061 = SHAPE_REPRESENTATION ( 'Bearing', ( #1299 ), #5023 ) ;
#8062 = AXIS2_PLACEMENT_3D ( 'NONE', #5919, #4009, #128 ) ;
#8063 = DIRECTION ( 'NONE',  ( 0.000000000000000000, 0.000000000000000000, 1.000000000000000000 ) ) ;
#8064 = ORIENTED_EDGE ( 'NONE', *, *, #6929, .T. ) ;
#8065 = ORIENTED_EDGE ( 'NONE', *, *, #4825, .T. ) ;
#8066 = VECTOR ( 'NONE', #5272, 1000.000000000000000 ) ;
#8067 = AXIS2_PLACEMENT_3D ( 'NONE', #5307, #4625, #1345 ) ;
#8068 = ORIENTED_EDGE ( 'NONE', *, *, #7137, .T. ) ;
#8069 = DIRECTION ( 'NONE',  ( -0.000000000000000000, -0.000000000000000000, 1.000000000000000000 ) ) ;
#8070 = ORIENTED_EDGE ( 'NONE', *, *, #4685, .F. ) ;
#8071 = ORIENTED_EDGE ( 'NONE', *, *, #7704, .T. ) ;
#8072 = DIRECTION ( 'NONE',  ( 0.000000000000000000, -2.960594732333750610E-16, 1.000000000000000000 ) ) ;
#8073 = AXIS2_PLACEMENT_3D ( 'NONE', #5557, #2359, #1001 ) ;
#8074 = VECTOR ( 'NONE', #4350, 1000.000000000000000 ) ;
#8075 = APPLICATION_CONTEXT ( 'automotive_design' ) ;
#8076 = FACE_OUTER_BOUND ( 'NONE', #4110, .T. ) ;
#8077 = ORIENTED_EDGE ( 'NONE', *, *, #2174, .F. ) ;
#8078 = SURFACE_SIDE_STYLE ('',( #5507 ) ) ;
#8079 = CIRCLE ( 'NONE', #2098, 5.999999999999991118 ) ;
#8080 = EDGE_LOOP ( 'NONE', ( #6156, #7510, #1837 ) ) ;
#8081 = CARTESIAN_POINT ( 'NONE',  ( 0.000000000000000000, 0.000000000000000000, 20.00000000000000355 ) ) ;
#8082 = ADVANCED_FACE ( 'NONE', ( #3021 ), #8139, .T. ) ;
#8083 = DIRECTION ( 'NONE',  ( -1.000000000000000000, -0.000000000000000000, -0.000000000000000000 ) ) ;
#8084 = FACE_OUTER_BOUND ( 'NONE', #138, .T. ) ;
#8085 = VECTOR ( 'NONE', #5914, 1000.000000000000227 ) ;
#8086 = EDGE_LOOP ( 'NONE', ( #1385, #7037 ) ) ;
#8087 = ORIENTED_EDGE ( 'NONE', *, *, #3599, .F. ) ;
#8088 = CARTESIAN_POINT ( 'NONE',  ( 60.99999999999997868, -55.00000000000000711, -27.50000000000000000 ) ) ;
#8089 = LINE ( 'NONE', #2972, #74 ) ;
#8090 = ORIENTED_EDGE ( 'NONE', *, *, #1448, .F. ) ;
#8091 = PRODUCT_DEFINITION_SHAPE ( 'NONE', 'NONE',  #3522 ) ;
#8092 = DIRECTION ( 'NONE',  ( -0.000000000000000000, -1.632680918566406547E-16, 1.000000000000000000 ) ) ;
#8093 = EDGE_CURVE ( 'NONE', #381, #1826, #8187, .T. ) ;
#8094 = ORIENTED_EDGE ( 'NONE', *, *, #6490, .T. ) ;
#8095 = EDGE_CURVE ( 'NONE', #5603, #5439, #1086, .T. ) ;
#8096 = CYLINDRICAL_SURFACE ( 'NONE', #7183, 15.00000000000000178 ) ;
#8097 = UNCERTAINTY_MEASURE_WITH_UNIT (LENGTH_MEASURE( 1.000000000000000082E-05 ), #425, 'distance_accuracy_value', 'NONE');
#8098 = VERTEX_POINT ( 'NONE', #3192 ) ;
#8099 = CARTESIAN_POINT ( 'NONE',  ( 102.5000000000000000, 0.000000000000000000, 0.000000000000000000 ) ) ;
#8100 = ORIENTED_EDGE ( 'NONE', *, *, #7106, .T. ) ;
#8101 = LINE ( 'NONE', #6827, #2682 ) ;
#8102 = VECTOR ( 'NONE', #4456, 1000.000000000000000 ) ;
#8103 = ORIENTED_EDGE ( 'NONE', *, *, #1636, .T. ) ;
#8104 = PLANE ( 'NONE',  #5931 ) ;
#8105 = EDGE_CURVE ( 'NONE', #2961, #7369, #5053, .T. ) ;
#8106 = VERTEX_POINT ( 'NONE', #6327 ) ;
#8107 = CYLINDRICAL_SURFACE ( 'NONE', #1054, 57.99999999999995737 ) ;
#8108 = CONICAL_SURFACE ( 'NONE', #1244, 4.999999999999990230, 1.029744258676653201 ) ;
#8109 = CARTESIAN_POINT ( 'NONE',  ( 0.000000000000000000, 125.0000000000000000, -12.50000000000000000 ) ) ;
#8110 = DIRECTION ( 'NONE',  ( -1.000000000000000000, 0.000000000000000000, 0.000000000000000000 ) ) ;
#8111 = ORIENTED_EDGE ( 'NONE', *, *, #5761, .T. ) ;
#8112 = ORIENTED_EDGE ( 'NONE', *, *, #3746, .T. ) ;
#8113 = ORIENTED_EDGE ( 'NONE', *, *, #7743, .T. ) ;
#8114 = CARTESIAN_POINT ( 'NONE',  ( 95.00000000000000000, 95.00000000000008527, 35.00000000000000000 ) ) ;
#8115 = AXIS2_PLACEMENT_3D ( 'NONE', #5888, #58, #5218 ) ;
#8116 = CARTESIAN_POINT ( 'NONE',  ( 49.00000000000000711, -55.00000000000000711, -27.50000000000000000 ) ) ;
#8117 = CARTESIAN_POINT ( 'NONE',  ( -4.420576121828486471, -49.80565028682020312, -0.8005904993895454069 ) ) ;
#8118 = SHAPE_REPRESENTATION_RELATIONSHIP ( 'NONE' , 'NONE' ,  #3965, #7639 ) ;
#8119 = ORIENTED_EDGE ( 'NONE', *, *, #2723, .F. ) ;
#8120 = CARTESIAN_POINT ( 'NONE',  ( 115.0000000000000000, 114.9999999999999716, 10.00000000000000000 ) ) ;
#8121 = PRODUCT_DEFINITION_FORMATION_WITH_SPECIFIED_SOURCE ( 'ANY', '', #2884, .NOT_KNOWN. ) ;
#8122 = DIRECTION ( 'NONE',  ( 1.000000000000000000, 0.000000000000000000, 0.000000000000000000 ) ) ;
#8123 =( REPRESENTATION_RELATIONSHIP ('NONE','NONE', #6882, #8061 ) REPRESENTATION_RELATIONSHIP_WITH_TRANSFORMATION ( #4535 )SHAPE_REPRESENTATION_RELATIONSHIP( ) );
#8124 = CARTESIAN_POINT ( 'NONE',  ( -75.00000000000001421, 0.000000000000000000, 57.99999999999999289 ) ) ;
#8125 = VERTEX_POINT ( 'NONE', #630 ) ;
#8126 = CARTESIAN_POINT ( 'NONE',  ( 0.000000000000000000, 37.49999999999999289, -250.0000000000000000 ) ) ;
#8127 = DIRECTION ( 'NONE',  ( -0.000000000000000000, -0.000000000000000000, 1.000000000000000000 ) ) ;
#8128 = EDGE_CURVE ( 'NONE', #1662, #3864, #7418, .T. ) ;
#8129 = FACE_OUTER_BOUND ( 'NONE', #7617, .T. ) ;
#8130 = PLANE ( 'NONE',  #563 ) ;
#8131 = DIRECTION ( 'NONE',  ( -1.000000000000000000, -0.000000000000000000, -0.000000000000000000 ) ) ;
#8132 = CIRCLE ( 'NONE', #3956, 5.499999999999991118 ) ;
#8133 = ORIENTED_EDGE ( 'NONE', *, *, #4995, .F. ) ;
#8134 = LINE ( 'NONE', #6098, #367 ) ;
#8135 = EDGE_CURVE ( 'NONE', #7887, #7809, #6467, .T. ) ;
#8136 = FACE_BOUND ( 'NONE', #2469, .T. ) ;
#8137 = ORIENTED_EDGE ( 'NONE', *, *, #973, .T. ) ;
#8138 = CARTESIAN_POINT ( 'NONE',  ( 95.00000000000000000, 95.00000000000008527, 70.00000000000000000 ) ) ;
#8139 = PLANE ( 'NONE',  #3625 ) ;
#8140 = EDGE_CURVE ( 'NONE', #1878, #5670, #3874, .T. ) ;
#8141 = ORIENTED_EDGE ( 'NONE', *, *, #1135, .T. ) ;
#8142 = AXIS2_PLACEMENT_3D ( 'NONE', #159, #7710, #1928 ) ;
#8143 = SHAPE_DEFINITION_REPRESENTATION ( #3786, #7203 ) ;
#8144 = ADVANCED_FACE ( 'NONE', ( #7002 ), #5182, .F. ) ;
#8145 = ADVANCED_FACE ( 'NONE', ( #1267 ), #1227, .F. ) ;
#8146 = VERTEX_POINT ( 'NONE', #5819 ) ;
#8147 = CARTESIAN_POINT ( 'NONE',  ( 125.0000000000000000, 120.0000000000000000, -28.00000000000002487 ) ) ;
#8148 = EDGE_LOOP ( 'NONE', ( #6304, #5992, #7344, #7150 ) ) ;
#8149 = DIRECTION ( 'NONE',  ( -1.000000000000000000, 0.000000000000000000, -0.000000000000000000 ) ) ;
#8150 = ORIENTED_EDGE ( 'NONE', *, *, #5152, .F. ) ;
#8151 = CYLINDRICAL_SURFACE ( 'NONE', #6575, 4.999999999999997335 ) ;
#8152 = VERTEX_POINT ( 'NONE', #5781 ) ;
#8153 = CARTESIAN_POINT ( 'NONE',  ( -114.9999999999999147, -100.0000000000000000, 250.0000000000000000 ) ) ;
#8154 = LINE ( 'NONE', #3411, #6666 ) ;
#8155 = CARTESIAN_POINT ( 'NONE',  ( 10.00000000000000000, 2.291769404546313661E-14, -93.74999999999998579 ) ) ;
#8156 = ORIENTED_EDGE ( 'NONE', *, *, #7686, .F. ) ;
#8157 = EDGE_CURVE ( 'NONE', #3656, #5937, #7781, .T. ) ;
#8158 = ORIENTED_EDGE ( 'NONE', *, *, #4266, .T. ) ;
#8159 = CIRCLE ( 'NONE', #7762, 4.171999999999999709 ) ;
#8160 = ORIENTED_EDGE ( 'NONE', *, *, #570, .F. ) ;
#8161 = CARTESIAN_POINT ( 'NONE',  ( -120.9999999999999005, 115.0000000000000000, 0.000000000000000000 ) ) ;
#8162 = FACE_OUTER_BOUND ( 'NONE', #837, .T. ) ;
#8163 = FACE_BOUND ( 'NONE', #1859, .T. ) ;
#8164 = PRODUCT_DEFINITION_SHAPE ( 'NONE', 'NONE',  #8368 ) ;
#8165 = CYLINDRICAL_SURFACE ( 'NONE', #2438, 4.999999999999990230 ) ;
#8166 = ORIENTED_EDGE ( 'NONE', *, *, #3635, .F. ) ;
#8167 = ADVANCED_FACE ( 'NONE', ( #2618 ), #4367, .F. ) ;
#8168 = CARTESIAN_POINT ( 'NONE',  ( -11.21327906667868390, -48.72680251680210972, -6.961169940684510671 ) ) ;
#8169 = EDGE_CURVE ( 'NONE', #6452, #7809, #3151, .T. ) ;
#8170 = ORIENTED_EDGE ( 'NONE', *, *, #6689, .F. ) ;
#8171 = ORIENTED_EDGE ( 'NONE', *, *, #190, .F. ) ;
#8172 = CARTESIAN_POINT ( 'NONE',  ( -125.0000000000000000, -125.0000000000000000, 340.0000000000000000 ) ) ;
#8173 = FACE_OUTER_BOUND ( 'NONE', #8036, .T. ) ;
#8174 = CARTESIAN_POINT ( 'NONE',  ( -110.0000000000000142, 115.0000000000000000, 270.0000000000000000 ) ) ;
#8175 = VERTEX_POINT ( 'NONE', #8319 ) ;
#8176 = LINE ( 'NONE', #915, #944 ) ;
#8177 = CARTESIAN_POINT ( 'NONE',  ( -115.0000000000000284, -115.0000000000000000, 20.00000000000000355 ) ) ;
#8178 = AXIS2_PLACEMENT_3D ( 'NONE', #7691, #4492, #1909 ) ;
#8179 = PLANE ( 'NONE',  #5769 ) ;
#8180 = AXIS2_PLACEMENT_3D ( 'NONE', #6668, #2213, #5239 ) ;
#8181 = DIRECTION ( 'NONE',  ( 1.000000000000000000, 0.000000000000000000, 0.000000000000000000 ) ) ;
#8182 = UNCERTAINTY_MEASURE_WITH_UNIT (LENGTH_MEASURE( 1.000000000000000082E-05 ), #4572, 'distance_accuracy_value', 'NONE');
#8183 = ORIENTED_EDGE ( 'NONE', *, *, #6434, .T. ) ;
#8184 = CARTESIAN_POINT ( 'NONE',  ( 10.40000000000000036, 0.000000000000000000, -5.400000000000035882 ) ) ;
#8185 = EDGE_LOOP ( 'NONE', ( #1948, #2465, #585, #641 ) ) ;
#8186 = CARTESIAN_POINT ( 'NONE',  ( 10.00000000000000000, -54.99999999999995026, -93.75000000000001421 ) ) ;
#8187 = LINE ( 'NONE', #548, #4714 ) ;
#8188 = AXIS2_PLACEMENT_3D ( 'NONE', #5719, #6421, #7761 ) ;
#8189 = ORIENTED_EDGE ( 'NONE', *, *, #7439, .T. ) ;
#8190 = CARTESIAN_POINT ( 'NONE',  ( 12.09737906851130873, 48.51474822866214964, -15.75174765218249284 ) ) ;
#8191 = VERTEX_POINT ( 'NONE', #5094 ) ;
#8192 = ORIENTED_EDGE ( 'NONE', *, *, #3525, .F. ) ;
#8193 = EDGE_CURVE ( 'NONE', #2674, #7479, #3564, .T. ) ;
#8194 = DIRECTION ( 'NONE',  ( 1.000000000000000000, 0.000000000000000000, 0.000000000000000000 ) ) ;
#8195 = VECTOR ( 'NONE', #1937, 1000.000000000000000 ) ;
#8196 = ORIENTED_EDGE ( 'NONE', *, *, #1285, .T. ) ;
#8197 = ORIENTED_EDGE ( 'NONE', *, *, #5260, .F. ) ;
#8198 = CARTESIAN_POINT ( 'NONE',  ( -1.236408833568031405E-20, 49.99999999999999289, -25.00000000000000000 ) ) ;
#8199 = DIRECTION ( 'NONE',  ( -0.000000000000000000, -0.000000000000000000, 1.000000000000000000 ) ) ;
#8200 = VECTOR ( 'NONE', #7999, 1000.000000000000000 ) ;
#8201 = CARTESIAN_POINT ( 'NONE',  ( -12.49987068959938519, 48.41232521539285472, -12.91614503987825024 ) ) ;
#8202 = ADVANCED_FACE ( 'NONE', ( #4451 ), #7044, .T. ) ;
#8203 = ORIENTED_EDGE ( 'NONE', *, *, #5918, .F. ) ;
#8204 = AXIS2_PLACEMENT_3D ( 'NONE', #6376, #2470, #4382 ) ;
#8205 = VERTEX_POINT ( 'NONE', #6399 ) ;
#8206 = AXIS2_PLACEMENT_3D ( 'NONE', #4146, #6909, #353 ) ;
#8207 = EDGE_CURVE ( 'NONE', #5352, #3543, #482, .T. ) ;
#8208 = EDGE_CURVE ( 'NONE', #6616, #3725, #7632, .T. ) ;
#8209 = DIRECTION ( 'NONE',  ( -1.000000000000000000, -0.000000000000000000, -0.000000000000000000 ) ) ;
#8210 = EDGE_CURVE ( 'NONE', #1618, #4379, #897, .T. ) ;
#8211 = COLOUR_RGB ( '',0.7921568627450980005, 0.8196078431372548767, 0.9333333333333333481 ) ;
#8212 = AXIS2_PLACEMENT_3D ( 'NONE', #804, #7257, #5278 ) ;
#8213 = CARTESIAN_POINT ( 'NONE',  ( 5.000000000000000000, 7.027796151710712813, -4.057500000000006324 ) ) ;
#8214 = LINE ( 'NONE', #7580, #633 ) ;
#8215 = SHAPE_REPRESENTATION_RELATIONSHIP ( 'NONE' , 'NONE' ,  #8061, #2227 ) ;
#8216 = CIRCLE ( 'NONE', #2790, 15.00000000000000000 ) ;
#8217 = VECTOR ( 'NONE', #7817, 1000.000000000000000 ) ;
#8218 = CIRCLE ( 'NONE', #5907, 54.99999999999996447 ) ;
#8219 = EDGE_CURVE ( 'NONE', #3826, #1534, #4659, .T. ) ;
#8220 = DIRECTION ( 'NONE',  ( 6.106226635438364917E-16, 3.154042683594196846E-17, 1.000000000000000000 ) ) ;
#8221 = DIRECTION ( 'NONE',  ( -0.000000000000000000, -0.000000000000000000, 1.000000000000000000 ) ) ;
#8222 = DIRECTION ( 'NONE',  ( -0.000000000000000000, -0.000000000000000000, -1.000000000000000000 ) ) ;
#8223 = EDGE_LOOP ( 'NONE', ( #3948, #414, #1241 ) ) ;
#8224 = CARTESIAN_POINT ( 'NONE',  ( 99.99999999999990052, 115.0000000000000000, 250.0000000000000000 ) ) ;
#8225 = EDGE_CURVE ( 'NONE', #5937, #6480, #8267, .T. ) ;
#8226 = DIRECTION ( 'NONE',  ( 1.000000000000000000, 1.040834085586084059E-15, 0.000000000000000000 ) ) ;
#8227 = ORIENTED_EDGE ( 'NONE', *, *, #3319, .T. ) ;
#8228 = DIRECTION ( 'NONE',  ( -0.000000000000000000, -0.000000000000000000, 1.000000000000000000 ) ) ;
#8229 = VECTOR ( 'NONE', #1841, 1000.000000000000000 ) ;
#8230 = CONICAL_SURFACE ( 'NONE', #6462, 4.057500000000000107, 1.047197551196592746 ) ;
#8231 = VERTEX_POINT ( 'NONE', #1941 ) ;
#8232 = CARTESIAN_POINT ( 'NONE',  ( 15.00000000000000000, 0.000000000000000000, -128.0000000000000284 ) ) ;
#8233 = CARTESIAN_POINT ( 'NONE',  ( 0.000000000000000000, 4.685197434473814759, -5.637851296924623057E-15 ) ) ;
#8234 = EDGE_LOOP ( 'NONE', ( #6994, #3958, #4255, #1083 ) ) ;
#8235 = CARTESIAN_POINT ( 'NONE',  ( -75.00000000000000000, 75.00000000000000000, 27.50000000000000000 ) ) ;
#8236 = CARTESIAN_POINT ( 'NONE',  ( 106.0000000000000142, -114.9999999999999716, 10.00000000000000000 ) ) ;
#8237 = SHAPE_DEFINITION_REPRESENTATION ( #3708, #3965 ) ;
#8238 = DIRECTION ( 'NONE',  ( -0.000000000000000000, -0.000000000000000000, 1.000000000000000000 ) ) ;
#8239 = PRODUCT_DEFINITION_SHAPE ( 'NONE', 'NONE',  #8370 ) ;
#8240 = VERTEX_POINT ( 'NONE', #2565 ) ;
#8241 = CARTESIAN_POINT ( 'NONE',  ( 124.9999999999997442, -125.0000000000000000, 0.000000000000000000 ) ) ;
#8242 = ORIENTED_EDGE ( 'NONE', *, *, #7608, .T. ) ;
#8243 = EDGE_LOOP ( 'NONE', ( #5790, #2448, #7637, #3554 ) ) ;
#8244 = CARTESIAN_POINT ( 'NONE',  ( -123.9999999999999716, 114.9999999999999858, 10.00000000000000000 ) ) ;
#8245 = DIRECTION ( 'NONE',  ( -0.000000000000000000, -0.000000000000000000, 1.000000000000000000 ) ) ;
#8246 = LINE ( 'NONE', #1953, #4683 ) ;
#8247 = EDGE_CURVE ( 'NONE', #15, #5855, #6354, .T. ) ;
#8248 = CARTESIAN_POINT ( 'NONE',  ( -11.22541203495697815, 48.72469304432832615, -18.06039341770851436 ) ) ;
#8249 = ORIENTED_EDGE ( 'NONE', *, *, #1655, .F. ) ;
#8250 = EDGE_LOOP ( 'NONE', ( #3701, #2054, #5729, #7814 ) ) ;
#8251 = LINE ( 'NONE', #4938, #1688 ) ;
#8252 = CYLINDRICAL_SURFACE ( 'NONE', #2677, 12.50000000000000000 ) ;
#8253 = DIRECTION ( 'NONE',  ( -1.000000000000000000, -1.321694076934710155E-16, -0.000000000000000000 ) ) ;
#8254 = ORIENTED_EDGE ( 'NONE', *, *, #5415, .F. ) ;
#8255 = DIRECTION ( 'NONE',  ( -0.000000000000000000, -0.000000000000000000, 1.000000000000000000 ) ) ;
#8256 = DIRECTION ( 'NONE',  ( 1.000000000000000000, 0.000000000000000000, 0.000000000000000000 ) ) ;
#8257 = EDGE_CURVE ( 'NONE', #7369, #4413, #3823, .T. ) ;
#8258 = EDGE_CURVE ( 'NONE', #1889, #5090, #1172, .T. ) ;
#8259 = ADVANCED_FACE ( 'NONE', ( #1291 ), #1258, .T. ) ;
#8260 = ORIENTED_EDGE ( 'NONE', *, *, #6024, .T. ) ;
#8261 = CARTESIAN_POINT ( 'NONE',  ( 5.000000000000000000, 3.513898075855365732, 2.028749999999995612 ) ) ;
#8262 = CARTESIAN_POINT ( 'NONE',  ( 0.000000000000000000, 125.0000000000000568, 66.99999999999992895 ) ) ;
#8263 = CARTESIAN_POINT ( 'NONE',  ( 106.0000000000000142, -114.9999999999999716, 20.00000000000000000 ) ) ;
#8264 = DIRECTION ( 'NONE',  ( -1.000000000000000000, 0.000000000000000000, -0.000000000000000000 ) ) ;
#8265 = LINE ( 'NONE', #7547, #3899 ) ;
#8266 = CARTESIAN_POINT ( 'NONE',  ( 2.854599402353564130, -49.92007443197287841, -0.3233859435660855763 ) ) ;
#8267 = LINE ( 'NONE', #6989, #1030 ) ;
#8268 = AXIS2_PLACEMENT_3D ( 'NONE', #1147, #6281, #6491 ) ;
#8269 = ADVANCED_FACE ( 'NONE', ( #576 ), #1337, .F. ) ;
#8270 = DIRECTION ( 'NONE',  ( 0.000000000000000000, 0.000000000000000000, -1.000000000000000000 ) ) ;
#8271 = EDGE_LOOP ( 'NONE', ( #3392, #4515 ) ) ;
#8272 = DIRECTION ( 'NONE',  ( -1.000000000000000000, -0.000000000000000000, -0.000000000000000000 ) ) ;
#8273 = AXIS2_PLACEMENT_3D ( 'NONE', #1296, #4506, #7060 ) ;
#8274 = VERTEX_POINT ( 'NONE', #2035 ) ;
#8275 = DIRECTION ( 'NONE',  ( 0.000000000000000000, -1.000000000000000000, 0.000000000000000000 ) ) ;
#8276 = VERTEX_POINT ( 'NONE', #6950 ) ;
#8277 = PRODUCT_DEFINITION_FORMATION_WITH_SPECIFIED_SOURCE ( 'ANY', '', #4297, .NOT_KNOWN. ) ;
#8278 = LINE ( 'NONE', #6273, #6174 ) ;
#8279 = DIRECTION ( 'NONE',  ( -0.000000000000000000, -0.000000000000000000, -1.000000000000000000 ) ) ;
#8280 = EDGE_LOOP ( 'NONE', ( #1230, #4333, #4769, #4153 ) ) ;
#8281 = CONTEXT_DEPENDENT_SHAPE_REPRESENTATION ( #4217, #3028 ) ;
#8282 = EDGE_CURVE ( 'NONE', #6062, #1706, #5874, .T. ) ;
#8283 = CARTESIAN_POINT ( 'NONE',  ( -1.236408833568031405E-20, 49.99999999999999289, -25.00000000000000000 ) ) ;
#8284 = CYLINDRICAL_SURFACE ( 'NONE', #6034, 12.99999999999999822 ) ;
#8285 = ORIENTED_EDGE ( 'NONE', *, *, #1636, .F. ) ;
#8286 = CARTESIAN_POINT ( 'NONE',  ( -114.9999999999999147, 115.0000000000000000, 0.000000000000000000 ) ) ;
#8287 = CIRCLE ( 'NONE', #38, 95.00000000000008527 ) ;
#8288 = VERTEX_POINT ( 'NONE', #3737 ) ;
#8289 = ORIENTED_EDGE ( 'NONE', *, *, #1015, .T. ) ;
#8290 = DIRECTION ( 'NONE',  ( -0.000000000000000000, -0.000000000000000000, 1.000000000000000000 ) ) ;
#8291 = AXIS2_PLACEMENT_3D ( 'NONE', #7057, #1278, #3844 ) ;
#8292 = EDGE_LOOP ( 'NONE', ( #514, #924 ) ) ;
#8293 = LINE ( 'NONE', #5114, #4257 ) ;
#8294 = FACE_OUTER_BOUND ( 'NONE', #1165, .T. ) ;
#8295 = ORIENTED_EDGE ( 'NONE', *, *, #6138, .T. ) ;
#8296 =( NAMED_UNIT ( * ) PLANE_ANGLE_UNIT ( ) SI_UNIT ( $, .RADIAN. ) );
#8297 = APPLICATION_CONTEXT ( 'automotive_design' ) ;
#8298 = ORIENTED_EDGE ( 'NONE', *, *, #2528, .F. ) ;
#8299 = EDGE_CURVE ( 'NONE', #5007, #210, #3178, .T. ) ;
#8300 = CARTESIAN_POINT ( 'NONE',  ( -54.99999999999999289, 55.00000000000000711, 27.50000000000000000 ) ) ;
#8301 = EDGE_CURVE ( 'NONE', #3725, #6102, #3855, .T. ) ;
#8302 = EDGE_CURVE ( 'NONE', #4245, #6339, #7727, .T. ) ;
#8303 = DIRECTION ( 'NONE',  ( 1.000000000000000000, 0.000000000000000000, 0.000000000000000000 ) ) ;
#8304 = DIRECTION ( 'NONE',  ( 6.106226635438361958E-16, 0.000000000000000000, 1.000000000000000000 ) ) ;
#8305 = CARTESIAN_POINT ( 'NONE',  ( 95.00000000000001421, 1.163414459189985801E-14, 0.000000000000000000 ) ) ;
#8306 = PRESENTATION_LAYER_ASSIGNMENT (  '', '', ( #7355 ) ) ;
#8307 = PRODUCT_DEFINITION_SHAPE ( 'NONE', 'NONE',  #8362 ) ;
#8308 = CARTESIAN_POINT ( 'NONE',  ( 10.00000000000000000, 54.99999999999995026, -93.74999999999997158 ) ) ;
#8309 = ORIENTED_EDGE ( 'NONE', *, *, #3134, .F. ) ;
#8310 = ORIENTED_EDGE ( 'NONE', *, *, #6299, .T. ) ;
#8311 = CIRCLE ( 'NONE', #1028, 12.50000000000000000 ) ;
#8312 = EDGE_CURVE ( 'NONE', #5271, #1665, #5746, .T. ) ;
#8313 = AXIS2_PLACEMENT_3D ( 'NONE', #2192, #5464, #4095 ) ;
#8314 = VERTEX_POINT ( 'NONE', #8305 ) ;
#8315 = LINE ( 'NONE', #6955, #2808 ) ;
#8316 = VECTOR ( 'NONE', #12, 1000.000000000000114 ) ;
#8317 = ORIENTED_EDGE ( 'NONE', *, *, #6752, .F. ) ;
#8318 = DIRECTION ( 'NONE',  ( -1.000000000000000000, 0.000000000000000000, 0.000000000000000000 ) ) ;
#8319 = CARTESIAN_POINT ( 'NONE',  ( -60.99999999999997868, -55.00000000000000711, -27.50000000000000000 ) ) ;
#8320 = ORIENTED_EDGE ( 'NONE', *, *, #3477, .T. ) ;
#8321 = ITEM_DEFINED_TRANSFORMATION ( 'NONE', 'NONE', #990,  #1299 ) ;
#8322 = CARTESIAN_POINT ( 'NONE',  ( 6.616553374552193389, 49.56145291835650823, -23.11303593919430099 ) ) ;
#8323 = VECTOR ( 'NONE', #4597, 1000.000000000000000 ) ;
#8324 = EDGE_CURVE ( 'NONE', #7479, #2674, #1703, .T. ) ;
#8325 = DIRECTION ( 'NONE',  ( -0.000000000000000000, -1.000000000000000000, 1.586032892321652236E-16 ) ) ;
#8326 = EDGE_CURVE ( 'NONE', #3745, #4377, #3171, .T. ) ;
#8327 = ORIENTED_EDGE ( 'NONE', *, *, #6301, .T. ) ;
#8328 = CARTESIAN_POINT ( 'NONE',  ( 125.0000000000000000, -125.0000000000000284, 70.00000000000000000 ) ) ;
#8329 = AXIS2_PLACEMENT_3D ( 'NONE', #699, #4477, #7028 ) ;
#8330 = DIRECTION ( 'NONE',  ( -1.000000000000000000, -0.000000000000000000, -0.000000000000000000 ) ) ;
#8331 = CIRCLE ( 'NONE', #1720, 5.999999999999991118 ) ;
#8332 = DIRECTION ( 'NONE',  ( -0.000000000000000000, -0.000000000000000000, -1.000000000000000000 ) ) ;
#8333 = DIRECTION ( 'NONE',  ( -0.000000000000000000, -0.000000000000000000, 1.000000000000000000 ) ) ;
#8334 = DIRECTION ( 'NONE',  ( 1.000000000000000000, 0.000000000000000000, 0.000000000000000000 ) ) ;
#8335 = ORIENTED_EDGE ( 'NONE', *, *, #1545, .F. ) ;
#8336 = SURFACE_STYLE_USAGE ( .BOTH. , #1163 ) ;
#8337 = DIRECTION ( 'NONE',  ( -0.9218685772373166332, 5.459367156011912432E-16, 0.3875026790906690444 ) ) ;
#8338 = CIRCLE ( 'NONE', #4679, 5.000000000000004441 ) ;
#8339 = VERTEX_POINT ( 'NONE', #3905 ) ;
#8340 = AXIS2_PLACEMENT_3D ( 'NONE', #6632, #4555, #7985 ) ;
#8341 = VERTEX_POINT ( 'NONE', #6473 ) ;
#8342 = DIRECTION ( 'NONE',  ( 0.000000000000000000, 0.000000000000000000, 1.000000000000000000 ) ) ;
#8343 = VECTOR ( 'NONE', #2327, 1000.000000000000114 ) ;
#8344 = CARTESIAN_POINT ( 'NONE',  ( -125.0000000000000000, 120.0000000000000000, -28.00000000000002487 ) ) ;
#8345 = DIRECTION ( 'NONE',  ( 0.8571673007021112234, 0.000000000000000000, 0.5150380749100560429 ) ) ;
#8346 = VECTOR ( 'NONE', #2655, 1000.000000000000000 ) ;
#8347 = LINE ( 'NONE', #6372, #793 ) ;
#8348 = NEXT_ASSEMBLY_USAGE_OCCURRENCE ( 'NAUO1', ' ', ' ', #6949, #557, $ ) ;
#8349 = NEXT_ASSEMBLY_USAGE_OCCURRENCE ( 'NAUO2', ' ', ' ', #6949, #2672, $ ) ;
#8350 = NEXT_ASSEMBLY_USAGE_OCCURRENCE ( 'NAUO3', ' ', ' ', #6949, #1585, $ ) ;
#8351 = NEXT_ASSEMBLY_USAGE_OCCURRENCE ( 'NAUO4', ' ', ' ', #6949, #969, $ ) ;
#8352 = NEXT_ASSEMBLY_USAGE_OCCURRENCE ( 'NAUO5', ' ', ' ', #6949, #969, $ ) ;
#8353 = NEXT_ASSEMBLY_USAGE_OCCURRENCE ( 'NAUO6', ' ', ' ', #6949, #4147, $ ) ;
#8354 = NEXT_ASSEMBLY_USAGE_OCCURRENCE ( 'NAUO7', ' ', ' ', #6949, #969, $ ) ;
#8355 = NEXT_ASSEMBLY_USAGE_OCCURRENCE ( 'NAUO8', ' ', ' ', #6949, #969, $ ) ;
#8356 = NEXT_ASSEMBLY_USAGE_OCCURRENCE ( 'NAUO9', ' ', ' ', #6949, #1686, $ ) ;
#8357 = NEXT_ASSEMBLY_USAGE_OCCURRENCE ( 'NAUO10', ' ', ' ', #6949, #7576, $ ) ;
#8358 = NEXT_ASSEMBLY_USAGE_OCCURRENCE ( 'NAUO11', ' ', ' ', #6949, #2910, $ ) ;
#8359 = NEXT_ASSEMBLY_USAGE_OCCURRENCE ( 'NAUO12', ' ', ' ', #6949, #2224, $ ) ;
#8360 = NEXT_ASSEMBLY_USAGE_OCCURRENCE ( 'NAUO13', ' ', ' ', #6949, #2224, $ ) ;
#8361 = NEXT_ASSEMBLY_USAGE_OCCURRENCE ( 'NAUO14', ' ', ' ', #6949, #3522, $ ) ;
#8362 = NEXT_ASSEMBLY_USAGE_OCCURRENCE ( 'NAUO15', ' ', ' ', #6949, #3522, $ ) ;
#8363 = NEXT_ASSEMBLY_USAGE_OCCURRENCE ( 'NAUO16', ' ', ' ', #6949, #3522, $ ) ;
#8364 = NEXT_ASSEMBLY_USAGE_OCCURRENCE ( 'NAUO17', ' ', ' ', #6949, #3522, $ ) ;
#8365 = NEXT_ASSEMBLY_USAGE_OCCURRENCE ( 'NAUO18', ' ', ' ', #6949, #3522, $ ) ;
#8366 = NEXT_ASSEMBLY_USAGE_OCCURRENCE ( 'NAUO19', ' ', ' ', #6949, #3522, $ ) ;
#8367 = NEXT_ASSEMBLY_USAGE_OCCURRENCE ( 'NAUO20', ' ', ' ', #6949, #3522, $ ) ;
#8368 = NEXT_ASSEMBLY_USAGE_OCCURRENCE ( 'NAUO21', ' ', ' ', #6949, #3522, $ ) ;
#8369 = NEXT_ASSEMBLY_USAGE_OCCURRENCE ( 'NAUO22', ' ', ' ', #6949, #3522, $ ) ;
#8370 = NEXT_ASSEMBLY_USAGE_OCCURRENCE ( 'NAUO23', ' ', ' ', #6949, #3522, $ ) ;
#8371 = NEXT_ASSEMBLY_USAGE_OCCURRENCE ( 'NAUO24', ' ', ' ', #6949, #3522, $ ) ;
#8372 = NEXT_ASSEMBLY_USAGE_OCCURRENCE ( 'NAUO25', ' ', ' ', #6949, #3522, $ ) ;
#8373=COLOUR_RGB('Dark Blue',0.08,0.2,0.34);
#8374=FILL_AREA_STYLE_COLOUR('',#8373);
#8375=FILL_AREA_STYLE('',(#8374));
#8376=SURFACE_STYLE_FILL_AREA(#8375);
#8377=SURFACE_SIDE_STYLE('',(#8376));
#8378=SURFACE_STYLE_USAGE(.BOTH.,#8377);
#8379=PRESENTATION_STYLE_ASSIGNMENT((#8378));
#8380=COLOUR_RGB('Light Blue',0.38,0.62,0.78);
#8381=FILL_AREA_STYLE_COLOUR('',#8380);
#8382=FILL_AREA_STYLE('',(#8381));
#8383=SURFACE_STYLE_FILL_AREA(#8382);
#8384=SURFACE_SIDE_STYLE('',(#8383));
#8385=SURFACE_STYLE_USAGE(.BOTH.,#8384);
#8386=PRESENTATION_STYLE_ASSIGNMENT((#8385));
#8387=COLOUR_RGB('Sky Blue',0.24,0.69,0.87);
#8388=FILL_AREA_STYLE_COLOUR('',#8387);
#8389=FILL_AREA_STYLE('',(#8388));
#8390=SURFACE_STYLE_FILL_AREA(#8389);
#8391=SURFACE_SIDE_STYLE('',(#8390));
#8392=SURFACE_STYLE_USAGE(.BOTH.,#8391);
#8393=PRESENTATION_STYLE_ASSIGNMENT((#8392));
#8394=COLOUR_RGB('Grey',0.48,0.52,0.57);
#8395=FILL_AREA_STYLE_COLOUR('',#8394);
#8396=FILL_AREA_STYLE('',(#8395));
#8397=SURFACE_STYLE_FILL_AREA(#8396);
#8398=SURFACE_SIDE_STYLE('',(#8397));
#8399=SURFACE_STYLE_USAGE(.BOTH.,#8398);
#8400=PRESENTATION_STYLE_ASSIGNMENT((#8399));
#8401=COLOUR_RGB('Black',0.12,0.14,0.17);
#8402=FILL_AREA_STYLE_COLOUR('',#8401);
#8403=FILL_AREA_STYLE('',(#8402));
#8404=SURFACE_STYLE_FILL_AREA(#8403);
#8405=SURFACE_SIDE_STYLE('',(#8404));
#8406=SURFACE_STYLE_USAGE(.BOTH.,#8405);
#8407=PRESENTATION_STYLE_ASSIGNMENT((#8406));
#8408=COLOUR_RGB('Off White',0.89,0.88,0.83);
#8409=FILL_AREA_STYLE_COLOUR('',#8408);
#8410=FILL_AREA_STYLE('',(#8409));
#8411=SURFACE_STYLE_FILL_AREA(#8410);
#8412=SURFACE_SIDE_STYLE('',(#8411));
#8413=SURFACE_STYLE_USAGE(.BOTH.,#8412);
#8414=PRESENTATION_STYLE_ASSIGNMENT((#8413));
ENDSEC;
END-ISO-10303-21;
